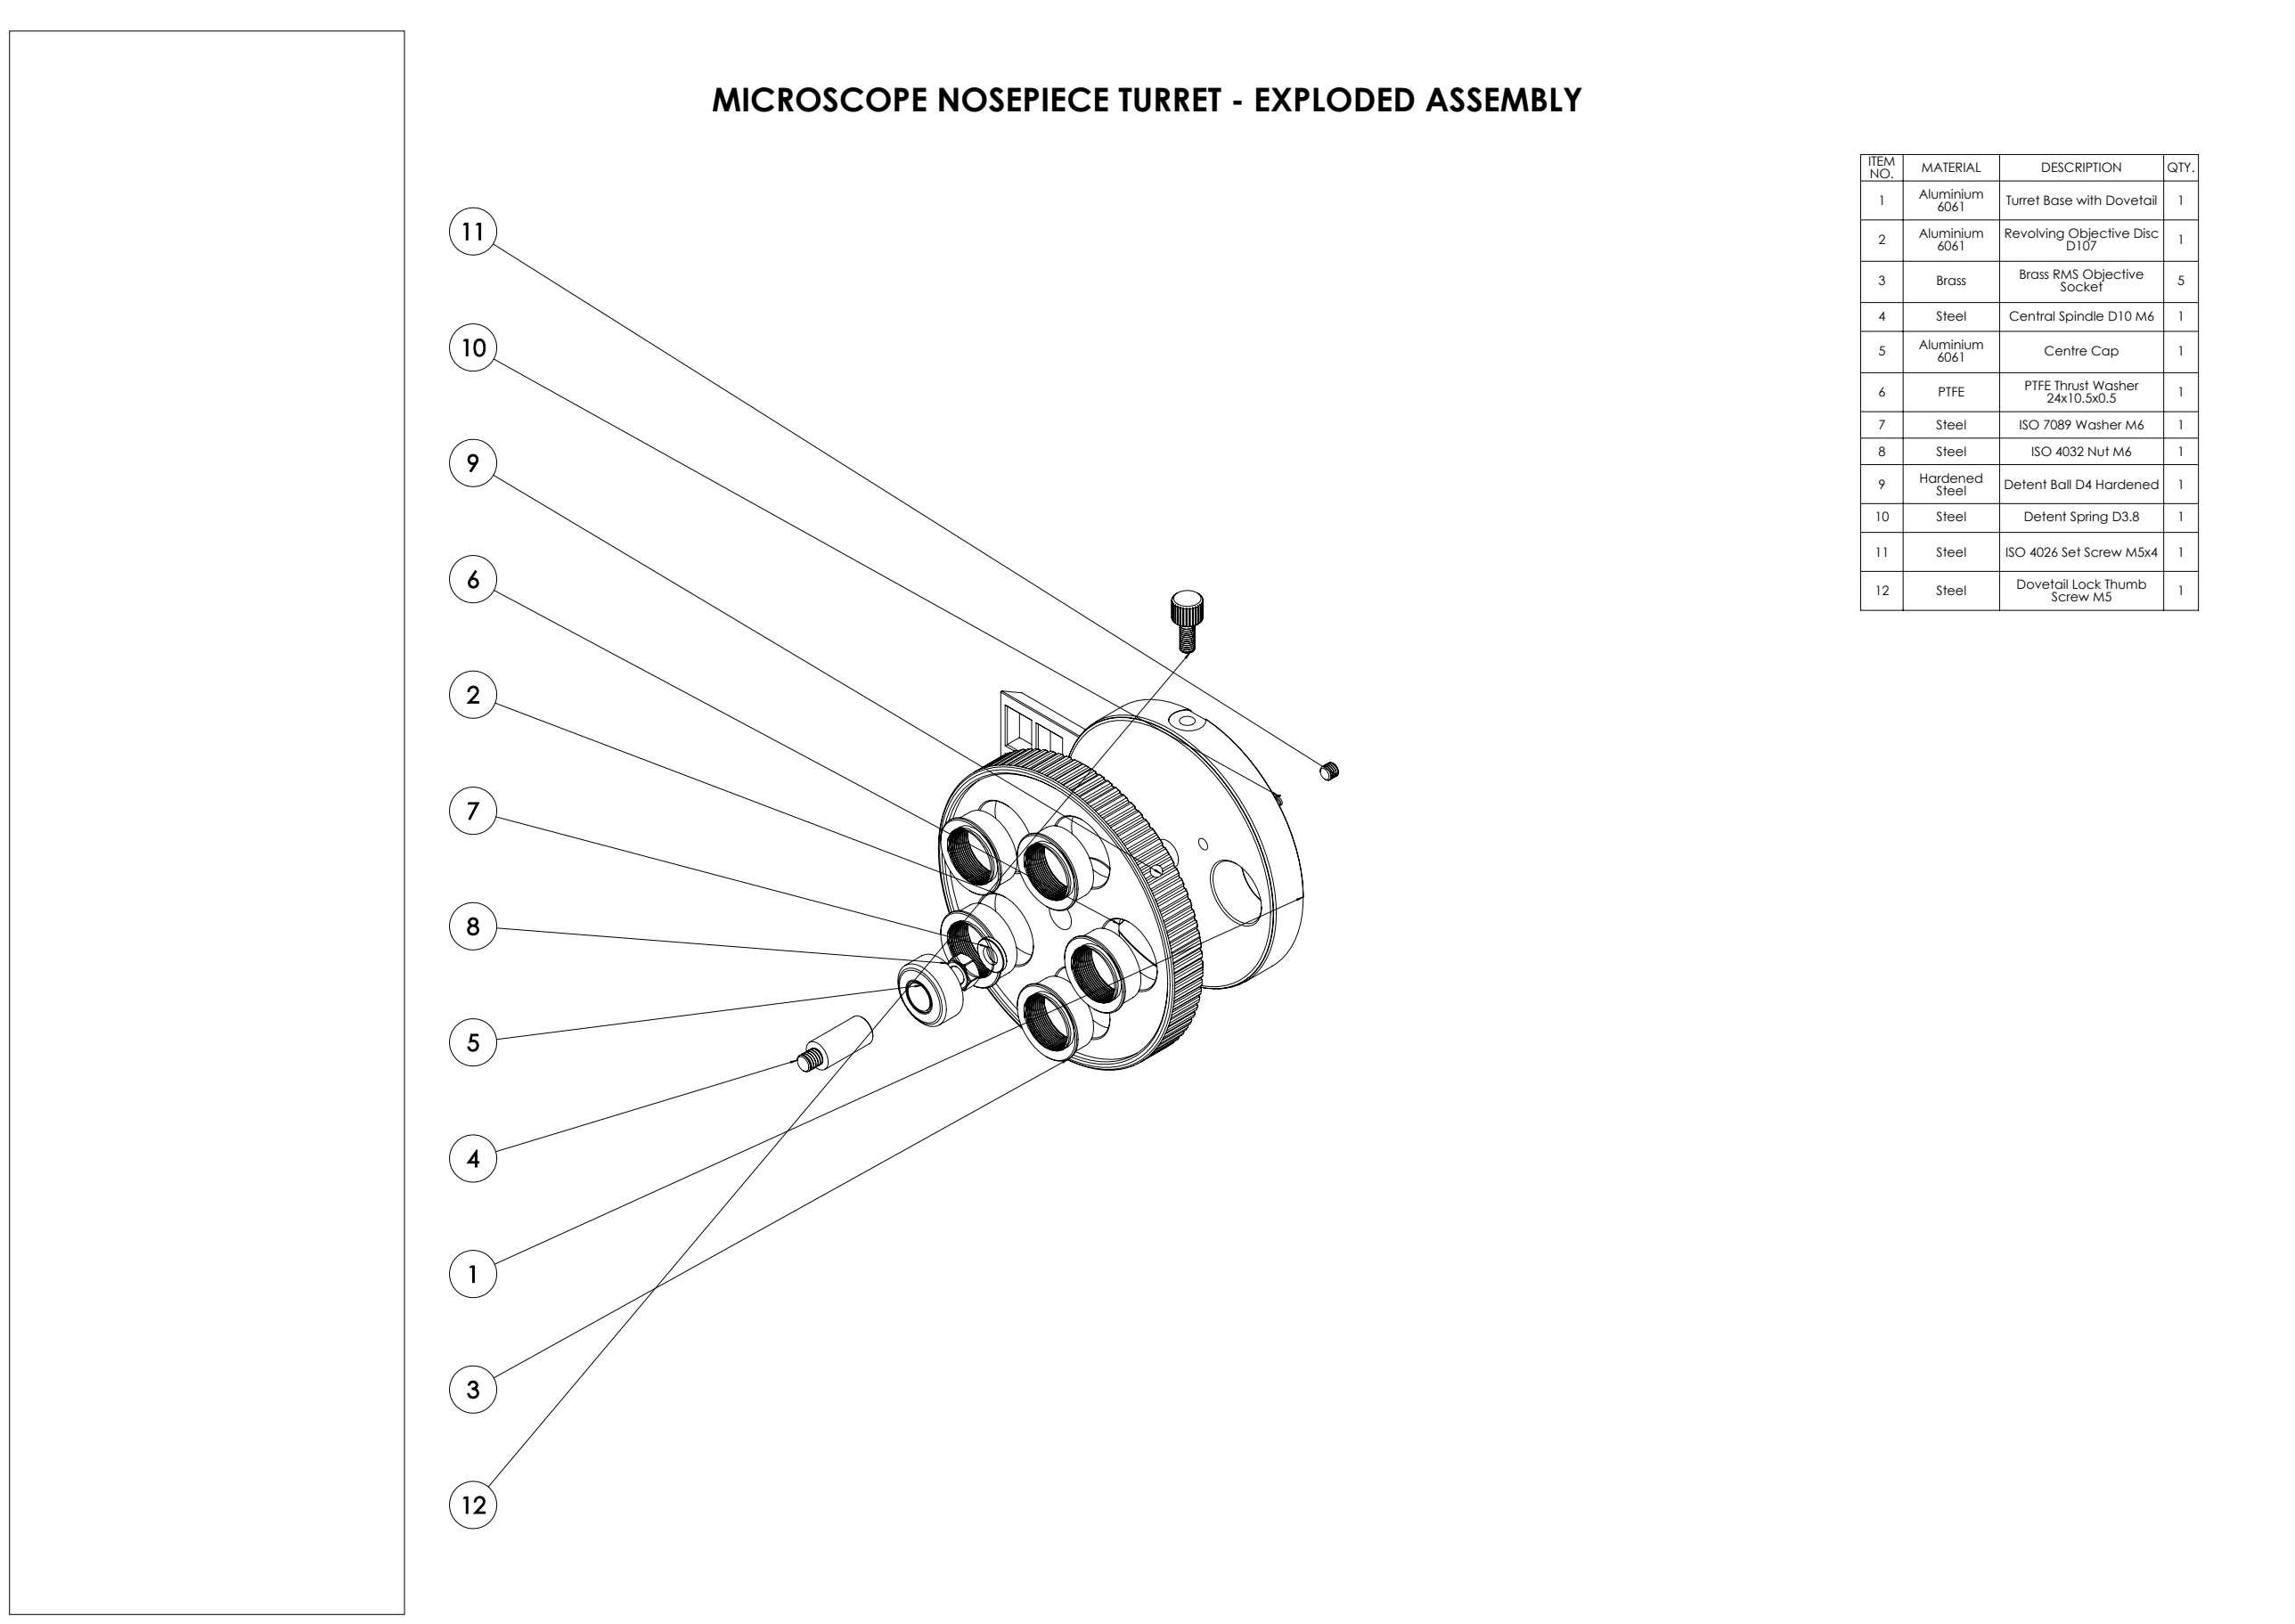
ISO-10303-21;
HEADER;
/* Generated by software containing ST-Developer
 * from STEP Tools, Inc. (www.steptools.com) 
 */

FILE_DESCRIPTION(
/* description */ (''),
/* implementation_level */ '2;1');

FILE_NAME(
/* name */ 'MAS-288',
/* time_stamp */ '2026-10-21T02:03:06-07:00',
/* author */ (''),
/* organization */ (''),
/* preprocessor_version */ 'ST-DEVELOPER v20.2',
/* originating_system */ 'Autodesk Translation Framework v15.15.0.0',
/* authorisation */ '');

FILE_SCHEMA (('AUTOMOTIVE_DESIGN { 1 0 10303 214 3 1 1 }'));
ENDSEC;

DATA;
#10=MECHANICAL_DESIGN_GEOMETRIC_PRESENTATION_REPRESENTATION('',(#115,#116,
#117,#118,#119,#120,#121,#122,#123,#124,#125,#126),#38528);
#11=ITEM_DEFINED_TRANSFORMATION($,$,#17218,#19009);
#12=ITEM_DEFINED_TRANSFORMATION($,$,#17323,#19010);
#13=ITEM_DEFINED_TRANSFORMATION($,$,#18599,#19011);
#14=ITEM_DEFINED_TRANSFORMATION($,$,#18599,#19012);
#15=ITEM_DEFINED_TRANSFORMATION($,$,#18599,#19013);
#16=ITEM_DEFINED_TRANSFORMATION($,$,#18599,#19014);
#17=ITEM_DEFINED_TRANSFORMATION($,$,#18599,#19015);
#18=ITEM_DEFINED_TRANSFORMATION($,$,#18641,#19016);
#19=ITEM_DEFINED_TRANSFORMATION($,$,#18673,#19017);
#20=ITEM_DEFINED_TRANSFORMATION($,$,#18699,#19018);
#21=ITEM_DEFINED_TRANSFORMATION($,$,#18708,#19019);
#22=ITEM_DEFINED_TRANSFORMATION($,$,#18722,#19020);
#23=ITEM_DEFINED_TRANSFORMATION($,$,#18766,#19021);
#24=ITEM_DEFINED_TRANSFORMATION($,$,#18769,#19022);
#25=ITEM_DEFINED_TRANSFORMATION($,$,#18774,#19023);
#26=ITEM_DEFINED_TRANSFORMATION($,$,#18808,#19024);
#27=(
REPRESENTATION_RELATIONSHIP($,$,#38576,#38575)
REPRESENTATION_RELATIONSHIP_WITH_TRANSFORMATION(#11)
SHAPE_REPRESENTATION_RELATIONSHIP()
);
#28=(
REPRESENTATION_RELATIONSHIP($,$,#38577,#38575)
REPRESENTATION_RELATIONSHIP_WITH_TRANSFORMATION(#12)
SHAPE_REPRESENTATION_RELATIONSHIP()
);
#29=(
REPRESENTATION_RELATIONSHIP($,$,#38578,#38575)
REPRESENTATION_RELATIONSHIP_WITH_TRANSFORMATION(#13)
SHAPE_REPRESENTATION_RELATIONSHIP()
);
#30=(
REPRESENTATION_RELATIONSHIP($,$,#38578,#38575)
REPRESENTATION_RELATIONSHIP_WITH_TRANSFORMATION(#14)
SHAPE_REPRESENTATION_RELATIONSHIP()
);
#31=(
REPRESENTATION_RELATIONSHIP($,$,#38578,#38575)
REPRESENTATION_RELATIONSHIP_WITH_TRANSFORMATION(#15)
SHAPE_REPRESENTATION_RELATIONSHIP()
);
#32=(
REPRESENTATION_RELATIONSHIP($,$,#38578,#38575)
REPRESENTATION_RELATIONSHIP_WITH_TRANSFORMATION(#16)
SHAPE_REPRESENTATION_RELATIONSHIP()
);
#33=(
REPRESENTATION_RELATIONSHIP($,$,#38578,#38575)
REPRESENTATION_RELATIONSHIP_WITH_TRANSFORMATION(#17)
SHAPE_REPRESENTATION_RELATIONSHIP()
);
#34=(
REPRESENTATION_RELATIONSHIP($,$,#38579,#38575)
REPRESENTATION_RELATIONSHIP_WITH_TRANSFORMATION(#18)
SHAPE_REPRESENTATION_RELATIONSHIP()
);
#35=(
REPRESENTATION_RELATIONSHIP($,$,#38580,#38575)
REPRESENTATION_RELATIONSHIP_WITH_TRANSFORMATION(#19)
SHAPE_REPRESENTATION_RELATIONSHIP()
);
#36=(
REPRESENTATION_RELATIONSHIP($,$,#38581,#38575)
REPRESENTATION_RELATIONSHIP_WITH_TRANSFORMATION(#20)
SHAPE_REPRESENTATION_RELATIONSHIP()
);
#37=(
REPRESENTATION_RELATIONSHIP($,$,#38582,#38575)
REPRESENTATION_RELATIONSHIP_WITH_TRANSFORMATION(#21)
SHAPE_REPRESENTATION_RELATIONSHIP()
);
#38=(
REPRESENTATION_RELATIONSHIP($,$,#38583,#38575)
REPRESENTATION_RELATIONSHIP_WITH_TRANSFORMATION(#22)
SHAPE_REPRESENTATION_RELATIONSHIP()
);
#39=(
REPRESENTATION_RELATIONSHIP($,$,#38584,#38575)
REPRESENTATION_RELATIONSHIP_WITH_TRANSFORMATION(#23)
SHAPE_REPRESENTATION_RELATIONSHIP()
);
#40=(
REPRESENTATION_RELATIONSHIP($,$,#38585,#38575)
REPRESENTATION_RELATIONSHIP_WITH_TRANSFORMATION(#24)
SHAPE_REPRESENTATION_RELATIONSHIP()
);
#41=(
REPRESENTATION_RELATIONSHIP($,$,#38586,#38575)
REPRESENTATION_RELATIONSHIP_WITH_TRANSFORMATION(#25)
SHAPE_REPRESENTATION_RELATIONSHIP()
);
#42=(
REPRESENTATION_RELATIONSHIP($,$,#38587,#38575)
REPRESENTATION_RELATIONSHIP_WITH_TRANSFORMATION(#26)
SHAPE_REPRESENTATION_RELATIONSHIP()
);
#43=CONTEXT_DEPENDENT_SHAPE_REPRESENTATION(#27,#38559);
#44=CONTEXT_DEPENDENT_SHAPE_REPRESENTATION(#28,#38560);
#45=CONTEXT_DEPENDENT_SHAPE_REPRESENTATION(#29,#38561);
#46=CONTEXT_DEPENDENT_SHAPE_REPRESENTATION(#30,#38562);
#47=CONTEXT_DEPENDENT_SHAPE_REPRESENTATION(#31,#38563);
#48=CONTEXT_DEPENDENT_SHAPE_REPRESENTATION(#32,#38564);
#49=CONTEXT_DEPENDENT_SHAPE_REPRESENTATION(#33,#38565);
#50=CONTEXT_DEPENDENT_SHAPE_REPRESENTATION(#34,#38566);
#51=CONTEXT_DEPENDENT_SHAPE_REPRESENTATION(#35,#38567);
#52=CONTEXT_DEPENDENT_SHAPE_REPRESENTATION(#36,#38568);
#53=CONTEXT_DEPENDENT_SHAPE_REPRESENTATION(#37,#38569);
#54=CONTEXT_DEPENDENT_SHAPE_REPRESENTATION(#38,#38570);
#55=CONTEXT_DEPENDENT_SHAPE_REPRESENTATION(#39,#38571);
#56=CONTEXT_DEPENDENT_SHAPE_REPRESENTATION(#40,#38572);
#57=CONTEXT_DEPENDENT_SHAPE_REPRESENTATION(#41,#38573);
#58=CONTEXT_DEPENDENT_SHAPE_REPRESENTATION(#42,#38574);
#59=NEXT_ASSEMBLY_USAGE_OCCURRENCE('01_Turret_Base_with_Dovetail:1',
'01_Turret_Base_with_Dovetail:1','01_Turret_Base_with_Dovetail:1',#38589,
#38590,'01_Turret_Base_with_Dovetail:1');
#60=NEXT_ASSEMBLY_USAGE_OCCURRENCE('02_Revolving_Objective_Disc_D107:1',
'02_Revolving_Objective_Disc_D107:1',
'02_Revolving_Objective_Disc_D107:1',#38589,#38591,
'02_Revolving_Objective_Disc_D107:1');
#61=NEXT_ASSEMBLY_USAGE_OCCURRENCE('03_Brass_RMS_Objective_Socket:2',
'03_Brass_RMS_Objective_Socket:2','03_Brass_RMS_Objective_Socket:2',#38589,
#38592,'03_Brass_RMS_Objective_Socket:2');
#62=NEXT_ASSEMBLY_USAGE_OCCURRENCE('03_Brass_RMS_Objective_Socket:3',
'03_Brass_RMS_Objective_Socket:3','03_Brass_RMS_Objective_Socket:3',#38589,
#38592,'03_Brass_RMS_Objective_Socket:3');
#63=NEXT_ASSEMBLY_USAGE_OCCURRENCE('03_Brass_RMS_Objective_Socket:4',
'03_Brass_RMS_Objective_Socket:4','03_Brass_RMS_Objective_Socket:4',#38589,
#38592,'03_Brass_RMS_Objective_Socket:4');
#64=NEXT_ASSEMBLY_USAGE_OCCURRENCE('03_Brass_RMS_Objective_Socket:5',
'03_Brass_RMS_Objective_Socket:5','03_Brass_RMS_Objective_Socket:5',#38589,
#38592,'03_Brass_RMS_Objective_Socket:5');
#65=NEXT_ASSEMBLY_USAGE_OCCURRENCE('03_Brass_RMS_Objective_Socket:6',
'03_Brass_RMS_Objective_Socket:6','03_Brass_RMS_Objective_Socket:6',#38589,
#38592,'03_Brass_RMS_Objective_Socket:6');
#66=NEXT_ASSEMBLY_USAGE_OCCURRENCE('04_Central_Spindle_D10_M6:2',
'04_Central_Spindle_D10_M6:2','04_Central_Spindle_D10_M6:2',#38589,#38593,
'04_Central_Spindle_D10_M6:2');
#67=NEXT_ASSEMBLY_USAGE_OCCURRENCE('05_Centre_Cap:2','05_Centre_Cap:2',
'05_Centre_Cap:2',#38589,#38594,'05_Centre_Cap:2');
#68=NEXT_ASSEMBLY_USAGE_OCCURRENCE(
'06_PTFE_Thrust_Washer_24x10.5x0.5:2',
'06_PTFE_Thrust_Washer_24x10.5x0.5:2',
'06_PTFE_Thrust_Washer_24x10.5x0.5:2',#38589,#38595,
'06_PTFE_Thrust_Washer_24x10.5x0.5:2');
#69=NEXT_ASSEMBLY_USAGE_OCCURRENCE('07_ISO_7089_Washer_M6:2',
'07_ISO_7089_Washer_M6:2','07_ISO_7089_Washer_M6:2',#38589,#38596,
'07_ISO_7089_Washer_M6:2');
#70=NEXT_ASSEMBLY_USAGE_OCCURRENCE('08_ISO_4032_Nut_M6:2',
'08_ISO_4032_Nut_M6:2','08_ISO_4032_Nut_M6:2',#38589,#38597,
'08_ISO_4032_Nut_M6:2');
#71=NEXT_ASSEMBLY_USAGE_OCCURRENCE('09_Detent_Ball_D4_Hardened:2',
'09_Detent_Ball_D4_Hardened:2','09_Detent_Ball_D4_Hardened:2',#38589,#38598,
'09_Detent_Ball_D4_Hardened:2');
#72=NEXT_ASSEMBLY_USAGE_OCCURRENCE('10_Detent_Spring_D3.8:2',
'10_Detent_Spring_D3.8:2','10_Detent_Spring_D3.8:2',#38589,#38599,
'10_Detent_Spring_D3.8:2');
#73=NEXT_ASSEMBLY_USAGE_OCCURRENCE('11_ISO_4026_Set_Screw_M5x4:2',
'11_ISO_4026_Set_Screw_M5x4:2','11_ISO_4026_Set_Screw_M5x4:2',#38589,#38600,
'11_ISO_4026_Set_Screw_M5x4:2');
#74=NEXT_ASSEMBLY_USAGE_OCCURRENCE('12_Dovetail_Lock_Thumb_Screw_M5:2',
'12_Dovetail_Lock_Thumb_Screw_M5:2','12_Dovetail_Lock_Thumb_Screw_M5:2',
#38589,#38601,'12_Dovetail_Lock_Thumb_Screw_M5:2');
#75=SPHERICAL_SURFACE('',#18767,2.);
#76=B_SPLINE_SURFACE_WITH_KNOTS('',3,3,((#30041,#30042,#30043,#30044,#30045,
#30046,#30047,#30048,#30049,#30050,#30051,#30052,#30053,#30054,#30055,#30056,
#30057,#30058,#30059,#30060,#30061,#30062,#30063,#30064,#30065,#30066,#30067,
#30068,#30069,#30070,#30071,#30072,#30073,#30074,#30075,#30076,#30077,#30078,
#30079,#30080,#30081,#30082,#30083,#30084,#30085,#30086,#30087,#30088,#30089,
#30090,#30091,#30092,#30093,#30094,#30095,#30096,#30097,#30098,#30099,#30100,
#30101,#30102,#30103,#30104,#30105,#30106,#30107,#30108,#30109,#30110,#30111,
#30112,#30113,#30114,#30115,#30116,#30117,#30118,#30119,#30120,#30121,#30122,
#30123,#30124,#30125,#30126,#30127,#30128,#30129,#30130,#30131,#30132,#30133,
#30134,#30135,#30136,#30137,#30138,#30139,#30140,#30141,#30142,#30143,#30144,
#30145,#30146,#30147,#30148,#30149,#30150,#30151,#30152,#30153,#30154,#30155,
#30156,#30157,#30158,#30159,#30160,#30161,#30162,#30163,#30164,#30165,#30166,
#30167,#30168,#30169,#30170,#30171,#30172,#30173,#30174,#30175,#30176,#30177,
#30178,#30179,#30180,#30181,#30182,#30183,#30184,#30185,#30186,#30187,#30188,
#30189,#30190,#30191,#30192,#30193,#30194,#30195,#30196,#30197,#30198,#30199),
(#30200,#30201,#30202,#30203,#30204,#30205,#30206,#30207,#30208,#30209,
#30210,#30211,#30212,#30213,#30214,#30215,#30216,#30217,#30218,#30219,#30220,
#30221,#30222,#30223,#30224,#30225,#30226,#30227,#30228,#30229,#30230,#30231,
#30232,#30233,#30234,#30235,#30236,#30237,#30238,#30239,#30240,#30241,#30242,
#30243,#30244,#30245,#30246,#30247,#30248,#30249,#30250,#30251,#30252,#30253,
#30254,#30255,#30256,#30257,#30258,#30259,#30260,#30261,#30262,#30263,#30264,
#30265,#30266,#30267,#30268,#30269,#30270,#30271,#30272,#30273,#30274,#30275,
#30276,#30277,#30278,#30279,#30280,#30281,#30282,#30283,#30284,#30285,#30286,
#30287,#30288,#30289,#30290,#30291,#30292,#30293,#30294,#30295,#30296,#30297,
#30298,#30299,#30300,#30301,#30302,#30303,#30304,#30305,#30306,#30307,#30308,
#30309,#30310,#30311,#30312,#30313,#30314,#30315,#30316,#30317,#30318,#30319,
#30320,#30321,#30322,#30323,#30324,#30325,#30326,#30327,#30328,#30329,#30330,
#30331,#30332,#30333,#30334,#30335,#30336,#30337,#30338,#30339,#30340,#30341,
#30342,#30343,#30344,#30345,#30346,#30347,#30348,#30349,#30350,#30351,#30352,
#30353,#30354,#30355,#30356,#30357,#30358),(#30359,#30360,#30361,#30362,
#30363,#30364,#30365,#30366,#30367,#30368,#30369,#30370,#30371,#30372,#30373,
#30374,#30375,#30376,#30377,#30378,#30379,#30380,#30381,#30382,#30383,#30384,
#30385,#30386,#30387,#30388,#30389,#30390,#30391,#30392,#30393,#30394,#30395,
#30396,#30397,#30398,#30399,#30400,#30401,#30402,#30403,#30404,#30405,#30406,
#30407,#30408,#30409,#30410,#30411,#30412,#30413,#30414,#30415,#30416,#30417,
#30418,#30419,#30420,#30421,#30422,#30423,#30424,#30425,#30426,#30427,#30428,
#30429,#30430,#30431,#30432,#30433,#30434,#30435,#30436,#30437,#30438,#30439,
#30440,#30441,#30442,#30443,#30444,#30445,#30446,#30447,#30448,#30449,#30450,
#30451,#30452,#30453,#30454,#30455,#30456,#30457,#30458,#30459,#30460,#30461,
#30462,#30463,#30464,#30465,#30466,#30467,#30468,#30469,#30470,#30471,#30472,
#30473,#30474,#30475,#30476,#30477,#30478,#30479,#30480,#30481,#30482,#30483,
#30484,#30485,#30486,#30487,#30488,#30489,#30490,#30491,#30492,#30493,#30494,
#30495,#30496,#30497,#30498,#30499,#30500,#30501,#30502,#30503,#30504,#30505,
#30506,#30507,#30508,#30509,#30510,#30511,#30512,#30513,#30514,#30515,#30516,
#30517),(#30518,#30519,#30520,#30521,#30522,#30523,#30524,#30525,#30526,
#30527,#30528,#30529,#30530,#30531,#30532,#30533,#30534,#30535,#30536,#30537,
#30538,#30539,#30540,#30541,#30542,#30543,#30544,#30545,#30546,#30547,#30548,
#30549,#30550,#30551,#30552,#30553,#30554,#30555,#30556,#30557,#30558,#30559,
#30560,#30561,#30562,#30563,#30564,#30565,#30566,#30567,#30568,#30569,#30570,
#30571,#30572,#30573,#30574,#30575,#30576,#30577,#30578,#30579,#30580,#30581,
#30582,#30583,#30584,#30585,#30586,#30587,#30588,#30589,#30590,#30591,#30592,
#30593,#30594,#30595,#30596,#30597,#30598,#30599,#30600,#30601,#30602,#30603,
#30604,#30605,#30606,#30607,#30608,#30609,#30610,#30611,#30612,#30613,#30614,
#30615,#30616,#30617,#30618,#30619,#30620,#30621,#30622,#30623,#30624,#30625,
#30626,#30627,#30628,#30629,#30630,#30631,#30632,#30633,#30634,#30635,#30636,
#30637,#30638,#30639,#30640,#30641,#30642,#30643,#30644,#30645,#30646,#30647,
#30648,#30649,#30650,#30651,#30652,#30653,#30654,#30655,#30656,#30657,#30658,
#30659,#30660,#30661,#30662,#30663,#30664,#30665,#30666,#30667,#30668,#30669,
#30670,#30671,#30672,#30673,#30674,#30675,#30676)),.UNSPECIFIED.,.F.,.F.,
 .F.,(4,4),(4,1,1,1,1,1,1,1,1,1,1,1,1,1,1,1,1,1,1,1,1,1,1,1,1,1,1,1,1,1,
1,1,1,1,1,1,1,1,1,1,1,1,1,1,1,1,1,1,1,1,1,1,1,1,1,1,1,1,1,1,1,1,1,1,1,1,
1,1,1,1,1,1,1,1,1,1,1,1,1,1,1,1,1,1,1,1,1,1,1,1,1,1,1,1,1,1,1,1,1,1,1,1,
1,1,1,1,1,1,1,1,1,1,1,1,1,1,1,1,1,1,1,1,1,1,1,1,1,1,1,1,1,1,1,1,1,1,1,1,
1,1,1,1,1,1,1,1,1,1,1,1,1,1,1,1,1,1,4),(0.,0.0485551576388473),(11.8415763884111,
12.3379359869576,12.8342955855041,13.3306551840506,13.827014782597,14.3233743811435,
14.81973397969,15.3160935782364,15.8124531767829,16.3088127753294,16.8051723738759,
17.3015319724223,17.7978915709688,18.2942511695153,18.7906107680618,19.2869703666082,
19.7833299651547,20.2796895637012,20.7760491622476,21.2724087607941,21.7687683593406,
22.2651279578871,22.7614875564335,23.25784715498,23.7542067535265,24.2505663520729,
24.7469259506194,25.2432855491659,25.7396451477124,26.2360047462588,26.7323643448053,
27.2287239433518,27.7250835418983,28.2214431404447,28.7178027389912,29.2141623375377,
29.7105219360841,30.2068815346306,30.7032411331771,31.1996007317236,31.69596033027,
32.1923199288165,32.688679527363,33.1850391259094,33.6813987244559,34.1777583230024,
34.6741179215489,35.1704775200953,35.6668371186418,36.1631967171883,36.6595563157347,
37.1559159142812,37.6522755128277,38.1486351113742,38.6449947099206,39.1413543084671,
39.6377139070136,40.1340735055601,40.6304331041065,41.126792702653,41.6231523011995,
42.1195118997459,42.6158714982924,43.1122310968389,43.6085906953854,44.1049502939318,
44.6013098924783,45.0976694910248,45.5940290895712,46.0903886881177,46.5867482866642,
47.0831078852107,47.5794674837571,48.0758270823036,48.5721866808501,49.0685462793965,
49.564905877943,50.0612654764895,50.557625075036,51.0539846735824,51.5503442721289,
52.0467038706754,52.5430634692219,53.0394230677683,53.5357826663148,54.0321422648613,
54.5285018634077,55.0248614619542,55.5212210605007,56.0175806590472,56.5139402575936,
57.0102998561401,57.5066594546866,58.003019053233,58.4993786517795,58.995738250326,
59.4920978488725,59.9884574474189,60.4848170459654,60.9811766445119,61.4775362430584,
61.9738958416048,62.4702554401513,62.9666150386978,63.4629746372442,63.9593342357907,
64.4556938343372,64.9520534328837,65.4484130314301,65.9447726299766,66.4411322285231,
66.9374918270696,67.433851425616,67.9302110241625,68.426570622709,68.9229302212554,
69.4192898198019,69.9156494183484,70.4120090168948,70.9083686154413,71.4047282139878,
71.9010878125343,72.3974474110807,72.8938070096272,73.3901666081737,73.8865262067201,
74.3828858052666,74.8792454038131,75.3756050023596,75.871964600906,76.3683241994525,
76.864683797999,77.3610433965455,77.8574029950919,78.3537625936384,78.8501221921849,
79.3464817907313,79.8428413892778,80.3392009878243,80.8355605863708,81.3319201849172,
81.8282797834637,82.3246393820102,82.8209989805567,83.3173585791031,83.8137181776496,
84.3100777761961,84.8064373747425,85.302796973289,85.7991565718355,86.295516170382,
86.7918757689284,87.2882353674749,87.7845949660214,88.2809545645678,88.7773141631143,
89.2736737616608),.UNSPECIFIED.);
#77=B_SPLINE_SURFACE_WITH_KNOTS('',3,3,((#30959,#30960,#30961,#30962,#30963,
#30964,#30965,#30966,#30967,#30968,#30969,#30970,#30971,#30972,#30973,#30974,
#30975,#30976,#30977,#30978,#30979,#30980,#30981,#30982,#30983,#30984,#30985,
#30986,#30987,#30988,#30989,#30990,#30991,#30992,#30993,#30994,#30995,#30996,
#30997,#30998,#30999,#31000,#31001,#31002,#31003,#31004,#31005,#31006,#31007,
#31008,#31009,#31010,#31011,#31012,#31013,#31014,#31015,#31016,#31017,#31018,
#31019,#31020,#31021,#31022,#31023,#31024,#31025,#31026,#31027,#31028,#31029,
#31030,#31031,#31032,#31033,#31034,#31035,#31036,#31037,#31038,#31039,#31040,
#31041,#31042,#31043,#31044,#31045,#31046,#31047,#31048,#31049,#31050,#31051,
#31052,#31053,#31054,#31055,#31056,#31057,#31058,#31059,#31060,#31061,#31062,
#31063,#31064,#31065,#31066,#31067,#31068,#31069,#31070,#31071,#31072,#31073,
#31074,#31075,#31076,#31077,#31078,#31079,#31080,#31081,#31082,#31083,#31084,
#31085,#31086,#31087,#31088,#31089,#31090,#31091,#31092,#31093,#31094,#31095,
#31096,#31097,#31098,#31099,#31100,#31101,#31102,#31103,#31104,#31105,#31106,
#31107,#31108,#31109,#31110,#31111,#31112,#31113,#31114,#31115,#31116,#31117),
(#31118,#31119,#31120,#31121,#31122,#31123,#31124,#31125,#31126,#31127,
#31128,#31129,#31130,#31131,#31132,#31133,#31134,#31135,#31136,#31137,#31138,
#31139,#31140,#31141,#31142,#31143,#31144,#31145,#31146,#31147,#31148,#31149,
#31150,#31151,#31152,#31153,#31154,#31155,#31156,#31157,#31158,#31159,#31160,
#31161,#31162,#31163,#31164,#31165,#31166,#31167,#31168,#31169,#31170,#31171,
#31172,#31173,#31174,#31175,#31176,#31177,#31178,#31179,#31180,#31181,#31182,
#31183,#31184,#31185,#31186,#31187,#31188,#31189,#31190,#31191,#31192,#31193,
#31194,#31195,#31196,#31197,#31198,#31199,#31200,#31201,#31202,#31203,#31204,
#31205,#31206,#31207,#31208,#31209,#31210,#31211,#31212,#31213,#31214,#31215,
#31216,#31217,#31218,#31219,#31220,#31221,#31222,#31223,#31224,#31225,#31226,
#31227,#31228,#31229,#31230,#31231,#31232,#31233,#31234,#31235,#31236,#31237,
#31238,#31239,#31240,#31241,#31242,#31243,#31244,#31245,#31246,#31247,#31248,
#31249,#31250,#31251,#31252,#31253,#31254,#31255,#31256,#31257,#31258,#31259,
#31260,#31261,#31262,#31263,#31264,#31265,#31266,#31267,#31268,#31269,#31270,
#31271,#31272,#31273,#31274,#31275,#31276),(#31277,#31278,#31279,#31280,
#31281,#31282,#31283,#31284,#31285,#31286,#31287,#31288,#31289,#31290,#31291,
#31292,#31293,#31294,#31295,#31296,#31297,#31298,#31299,#31300,#31301,#31302,
#31303,#31304,#31305,#31306,#31307,#31308,#31309,#31310,#31311,#31312,#31313,
#31314,#31315,#31316,#31317,#31318,#31319,#31320,#31321,#31322,#31323,#31324,
#31325,#31326,#31327,#31328,#31329,#31330,#31331,#31332,#31333,#31334,#31335,
#31336,#31337,#31338,#31339,#31340,#31341,#31342,#31343,#31344,#31345,#31346,
#31347,#31348,#31349,#31350,#31351,#31352,#31353,#31354,#31355,#31356,#31357,
#31358,#31359,#31360,#31361,#31362,#31363,#31364,#31365,#31366,#31367,#31368,
#31369,#31370,#31371,#31372,#31373,#31374,#31375,#31376,#31377,#31378,#31379,
#31380,#31381,#31382,#31383,#31384,#31385,#31386,#31387,#31388,#31389,#31390,
#31391,#31392,#31393,#31394,#31395,#31396,#31397,#31398,#31399,#31400,#31401,
#31402,#31403,#31404,#31405,#31406,#31407,#31408,#31409,#31410,#31411,#31412,
#31413,#31414,#31415,#31416,#31417,#31418,#31419,#31420,#31421,#31422,#31423,
#31424,#31425,#31426,#31427,#31428,#31429,#31430,#31431,#31432,#31433,#31434,
#31435),(#31436,#31437,#31438,#31439,#31440,#31441,#31442,#31443,#31444,
#31445,#31446,#31447,#31448,#31449,#31450,#31451,#31452,#31453,#31454,#31455,
#31456,#31457,#31458,#31459,#31460,#31461,#31462,#31463,#31464,#31465,#31466,
#31467,#31468,#31469,#31470,#31471,#31472,#31473,#31474,#31475,#31476,#31477,
#31478,#31479,#31480,#31481,#31482,#31483,#31484,#31485,#31486,#31487,#31488,
#31489,#31490,#31491,#31492,#31493,#31494,#31495,#31496,#31497,#31498,#31499,
#31500,#31501,#31502,#31503,#31504,#31505,#31506,#31507,#31508,#31509,#31510,
#31511,#31512,#31513,#31514,#31515,#31516,#31517,#31518,#31519,#31520,#31521,
#31522,#31523,#31524,#31525,#31526,#31527,#31528,#31529,#31530,#31531,#31532,
#31533,#31534,#31535,#31536,#31537,#31538,#31539,#31540,#31541,#31542,#31543,
#31544,#31545,#31546,#31547,#31548,#31549,#31550,#31551,#31552,#31553,#31554,
#31555,#31556,#31557,#31558,#31559,#31560,#31561,#31562,#31563,#31564,#31565,
#31566,#31567,#31568,#31569,#31570,#31571,#31572,#31573,#31574,#31575,#31576,
#31577,#31578,#31579,#31580,#31581,#31582,#31583,#31584,#31585,#31586,#31587,
#31588,#31589,#31590,#31591,#31592,#31593,#31594)),.UNSPECIFIED.,.F.,.F.,
 .F.,(4,4),(4,1,1,1,1,1,1,1,1,1,1,1,1,1,1,1,1,1,1,1,1,1,1,1,1,1,1,1,1,1,
1,1,1,1,1,1,1,1,1,1,1,1,1,1,1,1,1,1,1,1,1,1,1,1,1,1,1,1,1,1,1,1,1,1,1,1,
1,1,1,1,1,1,1,1,1,1,1,1,1,1,1,1,1,1,1,1,1,1,1,1,1,1,1,1,1,1,1,1,1,1,1,1,
1,1,1,1,1,1,1,1,1,1,1,1,1,1,1,1,1,1,1,1,1,1,1,1,1,1,1,1,1,1,1,1,1,1,1,1,
1,1,1,1,1,1,1,1,1,1,1,1,1,1,1,1,1,1,4),(0.,0.0485551576388473),(14.3988838068023,
14.8952434053488,15.3916030038952,15.8879626024417,16.3843222009882,16.8806817995346,
17.3770413980811,17.8734009966276,18.3697605951741,18.8661201937205,19.362479792267,
19.8588393908135,20.3551989893599,20.8515585879064,21.3479181864529,21.8442777849994,
22.3406373835458,22.8369969820923,23.3333565806388,23.8297161791853,24.3260757777317,
24.8224353762782,25.3187949748247,25.8151545733711,26.3115141719176,26.8078737704641,
27.3042333690106,27.800592967557,28.2969525661035,28.79331216465,29.2896717631964,
29.7860313617429,30.2823909602894,30.7787505588359,31.2751101573823,31.7714697559288,
32.2678293544753,32.7641889530218,33.2605485515682,33.7569081501147,34.2532677486612,
34.7496273472076,35.2459869457541,35.7423465443006,36.2387061428471,36.7350657413935,
37.23142533994,37.7277849384865,38.2241445370329,38.7205041355794,39.2168637341259,
39.7132233326724,40.2095829312188,40.7059425297653,41.2023021283118,41.6986617268582,
42.1950213254047,42.6913809239512,43.1877405224977,43.6841001210441,44.1804597195906,
44.6768193181371,45.1731789166836,45.66953851523,46.1658981137765,46.662257712323,
47.1586173108694,47.6549769094159,48.1513365079624,48.6476961065089,49.1440557050553,
49.6404153036018,50.1367749021483,50.6331345006947,51.1294940992412,51.6258536977877,
52.1222132963342,52.6185728948806,53.1149324934271,53.6112920919736,54.1076516905201,
54.6040112890665,55.100370887613,55.5967304861595,56.0930900847059,56.5894496832524,
57.0858092817989,57.5821688803454,58.0785284788918,58.5748880774383,59.0712476759848,
59.5676072745312,60.0639668730777,60.5603264716242,61.0566860701707,61.5530456687171,
62.0494052672636,62.5457648658101,63.0421244643565,63.538484062903,64.0348436614495,
64.531203259996,65.0275628585424,65.5239224570889,66.0202820556354,66.5166416541819,
67.0130012527283,67.5093608512748,68.0057204498213,68.5020800483677,68.9984396469142,
69.4947992454607,69.9911588440072,70.4875184425536,70.9838780411001,71.4802376396466,
71.9765972381931,72.4729568367395,72.969316435286,73.4656760338325,73.9620356323789,
74.4583952309254,74.9547548294719,75.4511144280183,75.9474740265648,76.4438336251113,
76.9401932236578,77.4365528222042,77.9329124207507,78.4292720192972,78.9256316178437,
79.4219912163901,79.9183508149366,80.4147104134831,80.9110700120296,81.407429610576,
81.9037892091225,82.400148807669,82.8965084062154,83.3928680047619,83.8892276033084,
84.3855872018549,84.8819468004013,85.3783063989478,85.8746659974943,86.3710255960407,
86.8673851945872,87.3637447931337,87.8601043916802,88.3564639902266,88.8528235887731,
89.3491831873196,89.845542785866,90.3419023844125,90.838261982959,91.3346215815055,
91.8309811800519),.UNSPECIFIED.);
#78=B_SPLINE_SURFACE_WITH_KNOTS('',3,3,((#32507,#32508,#32509,#32510,#32511,
#32512,#32513,#32514,#32515,#32516,#32517,#32518,#32519,#32520,#32521,#32522,
#32523,#32524,#32525,#32526,#32527,#32528,#32529,#32530,#32531,#32532,#32533,
#32534,#32535,#32536,#32537,#32538,#32539,#32540,#32541,#32542,#32543,#32544,
#32545,#32546,#32547,#32548,#32549,#32550),(#32551,#32552,#32553,#32554,
#32555,#32556,#32557,#32558,#32559,#32560,#32561,#32562,#32563,#32564,#32565,
#32566,#32567,#32568,#32569,#32570,#32571,#32572,#32573,#32574,#32575,#32576,
#32577,#32578,#32579,#32580,#32581,#32582,#32583,#32584,#32585,#32586,#32587,
#32588,#32589,#32590,#32591,#32592,#32593,#32594),(#32595,#32596,#32597,
#32598,#32599,#32600,#32601,#32602,#32603,#32604,#32605,#32606,#32607,#32608,
#32609,#32610,#32611,#32612,#32613,#32614,#32615,#32616,#32617,#32618,#32619,
#32620,#32621,#32622,#32623,#32624,#32625,#32626,#32627,#32628,#32629,#32630,
#32631,#32632,#32633,#32634,#32635,#32636,#32637,#32638),(#32639,#32640,
#32641,#32642,#32643,#32644,#32645,#32646,#32647,#32648,#32649,#32650,#32651,
#32652,#32653,#32654,#32655,#32656,#32657,#32658,#32659,#32660,#32661,#32662,
#32663,#32664,#32665,#32666,#32667,#32668,#32669,#32670,#32671,#32672,#32673,
#32674,#32675,#32676,#32677,#32678,#32679,#32680,#32681,#32682)),
 .UNSPECIFIED.,.F.,.F.,.F.,(4,4),(4,1,1,1,1,1,1,1,1,1,1,1,1,1,1,1,1,1,1,
1,1,1,1,1,1,1,1,1,1,1,1,1,1,1,1,1,1,1,1,1,1,4),(0.,0.0658467982010769),
(8.30747755240109,9.28631108327433,10.2651446141476,11.2439781450208,12.2228116758941,
13.2016452067673,14.1804787376406,15.1593122685138,16.1381457993871,17.1169793302603,
18.0958128611336,19.0746463920068,20.05347992288,21.0323134537533,22.0111469846265,
22.9899805154998,23.968814046373,24.9476475772463,25.9264811081195,26.9053146389928,
27.884148169866,28.8629817007393,29.8418152316125,30.8206487624858,31.799482293359,
32.7783158242323,33.7571493551055,34.7359828859787,35.714816416852,36.6936499477252,
37.6724834785985,38.6513170094717,39.630150540345,40.6089840712182,41.5878176020915,
42.5666511329647,43.545484663838,44.5243181947112,45.5031517255845,46.4819852564577,
47.460818787331,48.4396523182042),.UNSPECIFIED.);
#79=B_SPLINE_SURFACE_WITH_KNOTS('',3,3,((#32811,#32812,#32813,#32814,#32815,
#32816,#32817,#32818,#32819,#32820,#32821,#32822,#32823,#32824,#32825,#32826,
#32827,#32828,#32829,#32830,#32831,#32832,#32833,#32834,#32835,#32836,#32837,
#32838,#32839,#32840,#32841,#32842,#32843,#32844,#32845,#32846,#32847,#32848,
#32849,#32850,#32851,#32852,#32853,#32854),(#32855,#32856,#32857,#32858,
#32859,#32860,#32861,#32862,#32863,#32864,#32865,#32866,#32867,#32868,#32869,
#32870,#32871,#32872,#32873,#32874,#32875,#32876,#32877,#32878,#32879,#32880,
#32881,#32882,#32883,#32884,#32885,#32886,#32887,#32888,#32889,#32890,#32891,
#32892,#32893,#32894,#32895,#32896,#32897,#32898),(#32899,#32900,#32901,
#32902,#32903,#32904,#32905,#32906,#32907,#32908,#32909,#32910,#32911,#32912,
#32913,#32914,#32915,#32916,#32917,#32918,#32919,#32920,#32921,#32922,#32923,
#32924,#32925,#32926,#32927,#32928,#32929,#32930,#32931,#32932,#32933,#32934,
#32935,#32936,#32937,#32938,#32939,#32940,#32941,#32942),(#32943,#32944,
#32945,#32946,#32947,#32948,#32949,#32950,#32951,#32952,#32953,#32954,#32955,
#32956,#32957,#32958,#32959,#32960,#32961,#32962,#32963,#32964,#32965,#32966,
#32967,#32968,#32969,#32970,#32971,#32972,#32973,#32974,#32975,#32976,#32977,
#32978,#32979,#32980,#32981,#32982,#32983,#32984,#32985,#32986)),
 .UNSPECIFIED.,.F.,.F.,.F.,(4,4),(4,1,1,1,1,1,1,1,1,1,1,1,1,1,1,1,1,1,1,
1,1,1,1,1,1,1,1,1,1,1,1,1,1,1,1,1,1,1,1,1,1,4),(0.,0.0658467982010769),
(11.6150328478183,12.5938663786915,13.5726999095648,14.551533440438,15.5303669713113,
16.5092005021845,17.4880340330578,18.466867563931,19.4457010948043,20.4245346256775,
21.4033681565508,22.382201687424,23.3610352182973,24.3398687491705,25.3187022800437,
26.297535810917,27.2763693417902,28.2552028726635,29.2340364035367,30.21286993441,
31.1917034652832,32.1705369961565,33.1493705270297,34.128204057903,35.1070375887762,
36.0858711196495,37.0647046505227,38.043538181396,39.0223717122692,40.0012052431424,
40.9800387740157,41.9588723048889,42.9377058357622,43.9165393666354,44.8953728975087,
45.8742064283819,46.8530399592552,47.8318734901284,48.8107070210017,49.7895405518749,
50.7683740827482,51.7472076136214),.UNSPECIFIED.);
#80=B_SPLINE_SURFACE_WITH_KNOTS('',3,3,((#33437,#33438,#33439,#33440,#33441),
(#33442,#33443,#33444,#33445,#33446),(#33447,#33448,#33449,#33450,#33451),
(#33452,#33453,#33454,#33455,#33456)),.UNSPECIFIED.,.F.,.F.,.F.,(4,4),(4,
1,4),(0.,1.),(0.0610870649866808,0.309114526274187,0.639817807990862),
 .UNSPECIFIED.);
#81=B_SPLINE_SURFACE_WITH_KNOTS('',3,3,((#33486,#33487,#33488,#33489,#33490),
(#33491,#33492,#33493,#33494,#33495),(#33496,#33497,#33498,#33499,#33500),
(#33501,#33502,#33503,#33504,#33505)),.UNSPECIFIED.,.F.,.F.,.F.,(4,4),(4,
1,4),(0.,1.),(0.0610870649866807,0.309114526274187,0.639817807990862),
 .UNSPECIFIED.);
#82=B_SPLINE_SURFACE_WITH_KNOTS('',3,3,((#33575,#33576,#33577,#33578,#33579),
(#33580,#33581,#33582,#33583,#33584),(#33585,#33586,#33587,#33588,#33589),
(#33590,#33591,#33592,#33593,#33594)),.UNSPECIFIED.,.F.,.F.,.F.,(4,4),(4,
1,4),(0.,1.),(0.061087064986681,0.309114526274187,0.639817807990862),
 .UNSPECIFIED.);
#83=B_SPLINE_SURFACE_WITH_KNOTS('',3,3,((#33668,#33669,#33670,#33671,#33672),
(#33673,#33674,#33675,#33676,#33677),(#33678,#33679,#33680,#33681,#33682),
(#33683,#33684,#33685,#33686,#33687)),.UNSPECIFIED.,.F.,.F.,.F.,(4,4),(4,
1,4),(0.,1.),(0.0610870649866801,0.309114526274187,0.639817807990862),
 .UNSPECIFIED.);
#84=B_SPLINE_SURFACE_WITH_KNOTS('',3,3,((#33701,#33702,#33703,#33704,#33705),
(#33706,#33707,#33708,#33709,#33710),(#33711,#33712,#33713,#33714,#33715),
(#33716,#33717,#33718,#33719,#33720)),.UNSPECIFIED.,.F.,.F.,.F.,(4,4),(4,
1,4),(0.,1.),(0.0610870649866807,0.391790346703356,0.639817807990862),
 .UNSPECIFIED.);
#85=B_SPLINE_SURFACE_WITH_KNOTS('',3,3,((#33742,#33743,#33744,#33745,#33746),
(#33747,#33748,#33749,#33750,#33751),(#33752,#33753,#33754,#33755,#33756),
(#33757,#33758,#33759,#33760,#33761)),.UNSPECIFIED.,.F.,.F.,.F.,(4,4),(4,
1,4),(0.,1.),(0.0610870649866804,0.309114526274187,0.639817807990861),
 .UNSPECIFIED.);
#86=B_SPLINE_SURFACE_WITH_KNOTS('',3,3,((#33827,#33828,#33829,#33830,#33831,
#33832,#33833,#33834,#33835,#33836,#33837,#33838,#33839,#33840,#33841,#33842,
#33843,#33844,#33845,#33846,#33847,#33848,#33849,#33850,#33851,#33852,#33853,
#33854,#33855,#33856,#33857,#33858,#33859,#33860,#33861,#33862,#33863,#33864,
#33865,#33866,#33867,#33868,#33869,#33870,#33871,#33872,#33873,#33874,#33875,
#33876,#33877,#33878,#33879,#33880,#33881,#33882,#33883,#33884,#33885,#33886,
#33887,#33888,#33889),(#33890,#33891,#33892,#33893,#33894,#33895,#33896,
#33897,#33898,#33899,#33900,#33901,#33902,#33903,#33904,#33905,#33906,#33907,
#33908,#33909,#33910,#33911,#33912,#33913,#33914,#33915,#33916,#33917,#33918,
#33919,#33920,#33921,#33922,#33923,#33924,#33925,#33926,#33927,#33928,#33929,
#33930,#33931,#33932,#33933,#33934,#33935,#33936,#33937,#33938,#33939,#33940,
#33941,#33942,#33943,#33944,#33945,#33946,#33947,#33948,#33949,#33950,#33951,
#33952),(#33953,#33954,#33955,#33956,#33957,#33958,#33959,#33960,#33961,
#33962,#33963,#33964,#33965,#33966,#33967,#33968,#33969,#33970,#33971,#33972,
#33973,#33974,#33975,#33976,#33977,#33978,#33979,#33980,#33981,#33982,#33983,
#33984,#33985,#33986,#33987,#33988,#33989,#33990,#33991,#33992,#33993,#33994,
#33995,#33996,#33997,#33998,#33999,#34000,#34001,#34002,#34003,#34004,#34005,
#34006,#34007,#34008,#34009,#34010,#34011,#34012,#34013,#34014,#34015),
(#34016,#34017,#34018,#34019,#34020,#34021,#34022,#34023,#34024,#34025,
#34026,#34027,#34028,#34029,#34030,#34031,#34032,#34033,#34034,#34035,#34036,
#34037,#34038,#34039,#34040,#34041,#34042,#34043,#34044,#34045,#34046,#34047,
#34048,#34049,#34050,#34051,#34052,#34053,#34054,#34055,#34056,#34057,#34058,
#34059,#34060,#34061,#34062,#34063,#34064,#34065,#34066,#34067,#34068,#34069,
#34070,#34071,#34072,#34073,#34074,#34075,#34076,#34077,#34078),(#34079,
#34080,#34081,#34082,#34083,#34084,#34085,#34086,#34087,#34088,#34089,#34090,
#34091,#34092,#34093,#34094,#34095,#34096,#34097,#34098,#34099,#34100,#34101,
#34102,#34103,#34104,#34105,#34106,#34107,#34108,#34109,#34110,#34111,#34112,
#34113,#34114,#34115,#34116,#34117,#34118,#34119,#34120,#34121,#34122,#34123,
#34124,#34125,#34126,#34127,#34128,#34129,#34130,#34131,#34132,#34133,#34134,
#34135,#34136,#34137,#34138,#34139,#34140,#34141),(#34142,#34143,#34144,
#34145,#34146,#34147,#34148,#34149,#34150,#34151,#34152,#34153,#34154,#34155,
#34156,#34157,#34158,#34159,#34160,#34161,#34162,#34163,#34164,#34165,#34166,
#34167,#34168,#34169,#34170,#34171,#34172,#34173,#34174,#34175,#34176,#34177,
#34178,#34179,#34180,#34181,#34182,#34183,#34184,#34185,#34186,#34187,#34188,
#34189,#34190,#34191,#34192,#34193,#34194,#34195,#34196,#34197,#34198,#34199,
#34200,#34201,#34202,#34203,#34204),(#34205,#34206,#34207,#34208,#34209,
#34210,#34211,#34212,#34213,#34214,#34215,#34216,#34217,#34218,#34219,#34220,
#34221,#34222,#34223,#34224,#34225,#34226,#34227,#34228,#34229,#34230,#34231,
#34232,#34233,#34234,#34235,#34236,#34237,#34238,#34239,#34240,#34241,#34242,
#34243,#34244,#34245,#34246,#34247,#34248,#34249,#34250,#34251,#34252,#34253,
#34254,#34255,#34256,#34257,#34258,#34259,#34260,#34261,#34262,#34263,#34264,
#34265,#34266,#34267),(#34268,#34269,#34270,#34271,#34272,#34273,#34274,
#34275,#34276,#34277,#34278,#34279,#34280,#34281,#34282,#34283,#34284,#34285,
#34286,#34287,#34288,#34289,#34290,#34291,#34292,#34293,#34294,#34295,#34296,
#34297,#34298,#34299,#34300,#34301,#34302,#34303,#34304,#34305,#34306,#34307,
#34308,#34309,#34310,#34311,#34312,#34313,#34314,#34315,#34316,#34317,#34318,
#34319,#34320,#34321,#34322,#34323,#34324,#34325,#34326,#34327,#34328,#34329,
#34330),(#34331,#34332,#34333,#34334,#34335,#34336,#34337,#34338,#34339,
#34340,#34341,#34342,#34343,#34344,#34345,#34346,#34347,#34348,#34349,#34350,
#34351,#34352,#34353,#34354,#34355,#34356,#34357,#34358,#34359,#34360,#34361,
#34362,#34363,#34364,#34365,#34366,#34367,#34368,#34369,#34370,#34371,#34372,
#34373,#34374,#34375,#34376,#34377,#34378,#34379,#34380,#34381,#34382,#34383,
#34384,#34385,#34386,#34387,#34388,#34389,#34390,#34391,#34392,#34393),
(#34394,#34395,#34396,#34397,#34398,#34399,#34400,#34401,#34402,#34403,
#34404,#34405,#34406,#34407,#34408,#34409,#34410,#34411,#34412,#34413,#34414,
#34415,#34416,#34417,#34418,#34419,#34420,#34421,#34422,#34423,#34424,#34425,
#34426,#34427,#34428,#34429,#34430,#34431,#34432,#34433,#34434,#34435,#34436,
#34437,#34438,#34439,#34440,#34441,#34442,#34443,#34444,#34445,#34446,#34447,
#34448,#34449,#34450,#34451,#34452,#34453,#34454,#34455,#34456),(#34457,
#34458,#34459,#34460,#34461,#34462,#34463,#34464,#34465,#34466,#34467,#34468,
#34469,#34470,#34471,#34472,#34473,#34474,#34475,#34476,#34477,#34478,#34479,
#34480,#34481,#34482,#34483,#34484,#34485,#34486,#34487,#34488,#34489,#34490,
#34491,#34492,#34493,#34494,#34495,#34496,#34497,#34498,#34499,#34500,#34501,
#34502,#34503,#34504,#34505,#34506,#34507,#34508,#34509,#34510,#34511,#34512,
#34513,#34514,#34515,#34516,#34517,#34518,#34519)),.UNSPECIFIED.,.T.,.F.,
 .F.,(4,1,1,1,1,1,1,1,4),(4,1,1,1,1,1,1,1,1,1,1,1,1,1,1,1,1,1,1,1,1,1,1,
1,1,1,1,1,1,1,1,1,1,1,1,1,1,1,1,1,1,1,1,1,1,1,1,1,1,1,1,1,1,1,1,1,1,1,1,
1,4),(-3.14159265358979,-2.46839422782055,-2.24399475256414,-1.34639685153848,
-0.448798950512828,0.448798950512828,1.34639685153848,2.24399475256414,
3.14159265358979),(0.,0.00892857142857143,0.0178571428571429,0.0357142857142857,
0.0535714285714286,0.0714285714285714,0.0892857142857143,0.107142857142857,
0.125,0.142857142857143,0.154761904761905,0.166666666666667,0.178571428571429,
0.19047619047619,0.202380952380952,0.214285714285714,0.238095238095238,
0.261904761904762,0.273809523809524,0.285714285714286,0.30952380952381,
0.333333333333333,0.357142857142857,0.369047619047619,0.380952380952381,
0.392857142857143,0.404761904761905,0.416666666666667,0.428571428571429,
0.446428571428571,0.464285714285714,0.482142857142857,0.5,0.517857142857143,
0.535714285714286,0.553571428571429,0.571428571428571,0.589285714285714,
0.607142857142857,0.625,0.642857142857143,0.660714285714286,0.678571428571428,
0.696428571428571,0.714285714285714,0.726190476190476,0.738095238095238,
0.761904761904762,0.785714285714286,0.809523809523809,0.833333333333333,
0.857142857142857,0.875,0.892857142857143,0.910714285714286,0.928571428571429,
0.946428571428571,0.964285714285714,0.982142857142857,0.991071428571429,
1.),.UNSPECIFIED.);
#87=B_SPLINE_SURFACE_WITH_KNOTS('',3,3,((#35032,#35033,#35034,#35035,#35036,
#35037,#35038,#35039,#35040,#35041,#35042,#35043,#35044,#35045,#35046,#35047,
#35048,#35049,#35050,#35051,#35052,#35053,#35054,#35055,#35056,#35057,#35058,
#35059,#35060,#35061,#35062),(#35063,#35064,#35065,#35066,#35067,#35068,
#35069,#35070,#35071,#35072,#35073,#35074,#35075,#35076,#35077,#35078,#35079,
#35080,#35081,#35082,#35083,#35084,#35085,#35086,#35087,#35088,#35089,#35090,
#35091,#35092,#35093),(#35094,#35095,#35096,#35097,#35098,#35099,#35100,
#35101,#35102,#35103,#35104,#35105,#35106,#35107,#35108,#35109,#35110,#35111,
#35112,#35113,#35114,#35115,#35116,#35117,#35118,#35119,#35120,#35121,#35122,
#35123,#35124),(#35125,#35126,#35127,#35128,#35129,#35130,#35131,#35132,
#35133,#35134,#35135,#35136,#35137,#35138,#35139,#35140,#35141,#35142,#35143,
#35144,#35145,#35146,#35147,#35148,#35149,#35150,#35151,#35152,#35153,#35154,
#35155)),.UNSPECIFIED.,.F.,.F.,.F.,(4,4),(4,1,1,1,1,1,1,1,1,1,1,1,1,1,1,
1,1,1,1,1,1,1,1,1,1,1,1,1,4),(0.,0.0526254770366344),(8.30815772716268,
9.30733212220219,10.3065065172417,11.3056809122812,12.3048553073207,13.3040297023602,
14.3032040973997,15.3023784924392,16.3015528874787,17.3007272825182,18.2999016775577,
19.2990760725973,20.2982504676368,21.2974248626763,22.2965992577158,23.2957736527553,
24.2949480477948,25.2941224428343,26.2932968378738,27.2924712329133,28.2916456279528,
29.2908200229923,30.2899944180318,31.2891688130713,32.2883432081108,33.2875176031503,
34.2866919981899,35.2858663932294,36.2850407882689),.UNSPECIFIED.);
#88=B_SPLINE_SURFACE_WITH_KNOTS('',3,3,((#35379,#35380,#35381,#35382,#35383,
#35384,#35385,#35386,#35387,#35388,#35389,#35390,#35391,#35392,#35393,#35394,
#35395,#35396,#35397,#35398,#35399,#35400,#35401,#35402,#35403,#35404,#35405,
#35406,#35407,#35408,#35409),(#35410,#35411,#35412,#35413,#35414,#35415,
#35416,#35417,#35418,#35419,#35420,#35421,#35422,#35423,#35424,#35425,#35426,
#35427,#35428,#35429,#35430,#35431,#35432,#35433,#35434,#35435,#35436,#35437,
#35438,#35439,#35440),(#35441,#35442,#35443,#35444,#35445,#35446,#35447,
#35448,#35449,#35450,#35451,#35452,#35453,#35454,#35455,#35456,#35457,#35458,
#35459,#35460,#35461,#35462,#35463,#35464,#35465,#35466,#35467,#35468,#35469,
#35470,#35471),(#35472,#35473,#35474,#35475,#35476,#35477,#35478,#35479,
#35480,#35481,#35482,#35483,#35484,#35485,#35486,#35487,#35488,#35489,#35490,
#35491,#35492,#35493,#35494,#35495,#35496,#35497,#35498,#35499,#35500,#35501,
#35502)),.UNSPECIFIED.,.F.,.F.,.F.,(4,4),(4,1,1,1,1,1,1,1,1,1,1,1,1,1,1,
1,1,1,1,1,1,1,1,1,1,1,1,1,4),(0.,0.0526254770366344),(11.6163931973415,
12.615567592381,13.6147419874205,14.61391638246,15.6130907774995,16.612265172539,
17.6114395675785,18.610613962618,19.6097883576575,20.6089627526971,21.6081371477366,
22.6073115427761,23.6064859378156,24.6056603328551,25.6048347278946,26.6040091229341,
27.6031835179736,28.6023579130131,29.6015323080526,30.6007067030921,31.5998810981316,
32.5990554931711,33.5982298882106,34.5974042832501,35.5965786782897,36.5957530733292,
37.5949274683687,38.5941018634082,39.5932762584477),.UNSPECIFIED.);
#89=B_SPLINE_SURFACE_WITH_KNOTS('',3,3,((#36636,#36637,#36638,#36639,#36640,
#36641,#36642,#36643,#36644,#36645,#36646,#36647,#36648,#36649,#36650,#36651,
#36652,#36653,#36654,#36655,#36656,#36657,#36658,#36659,#36660,#36661,#36662,
#36663,#36664,#36665,#36666,#36667,#36668,#36669,#36670,#36671,#36672,#36673,
#36674,#36675,#36676,#36677,#36678,#36679,#36680,#36681,#36682,#36683,#36684,
#36685,#36686,#36687,#36688,#36689,#36690,#36691,#36692,#36693,#36694,#36695,
#36696,#36697,#36698,#36699,#36700,#36701,#36702,#36703,#36704,#36705,#36706,
#36707,#36708,#36709,#36710,#36711,#36712,#36713,#36714,#36715,#36716,#36717,
#36718,#36719,#36720,#36721,#36722,#36723,#36724,#36725,#36726,#36727,#36728,
#36729,#36730,#36731,#36732),(#36733,#36734,#36735,#36736,#36737,#36738,
#36739,#36740,#36741,#36742,#36743,#36744,#36745,#36746,#36747,#36748,#36749,
#36750,#36751,#36752,#36753,#36754,#36755,#36756,#36757,#36758,#36759,#36760,
#36761,#36762,#36763,#36764,#36765,#36766,#36767,#36768,#36769,#36770,#36771,
#36772,#36773,#36774,#36775,#36776,#36777,#36778,#36779,#36780,#36781,#36782,
#36783,#36784,#36785,#36786,#36787,#36788,#36789,#36790,#36791,#36792,#36793,
#36794,#36795,#36796,#36797,#36798,#36799,#36800,#36801,#36802,#36803,#36804,
#36805,#36806,#36807,#36808,#36809,#36810,#36811,#36812,#36813,#36814,#36815,
#36816,#36817,#36818,#36819,#36820,#36821,#36822,#36823,#36824,#36825,#36826,
#36827,#36828,#36829),(#36830,#36831,#36832,#36833,#36834,#36835,#36836,
#36837,#36838,#36839,#36840,#36841,#36842,#36843,#36844,#36845,#36846,#36847,
#36848,#36849,#36850,#36851,#36852,#36853,#36854,#36855,#36856,#36857,#36858,
#36859,#36860,#36861,#36862,#36863,#36864,#36865,#36866,#36867,#36868,#36869,
#36870,#36871,#36872,#36873,#36874,#36875,#36876,#36877,#36878,#36879,#36880,
#36881,#36882,#36883,#36884,#36885,#36886,#36887,#36888,#36889,#36890,#36891,
#36892,#36893,#36894,#36895,#36896,#36897,#36898,#36899,#36900,#36901,#36902,
#36903,#36904,#36905,#36906,#36907,#36908,#36909,#36910,#36911,#36912,#36913,
#36914,#36915,#36916,#36917,#36918,#36919,#36920,#36921,#36922,#36923,#36924,
#36925,#36926),(#36927,#36928,#36929,#36930,#36931,#36932,#36933,#36934,
#36935,#36936,#36937,#36938,#36939,#36940,#36941,#36942,#36943,#36944,#36945,
#36946,#36947,#36948,#36949,#36950,#36951,#36952,#36953,#36954,#36955,#36956,
#36957,#36958,#36959,#36960,#36961,#36962,#36963,#36964,#36965,#36966,#36967,
#36968,#36969,#36970,#36971,#36972,#36973,#36974,#36975,#36976,#36977,#36978,
#36979,#36980,#36981,#36982,#36983,#36984,#36985,#36986,#36987,#36988,#36989,
#36990,#36991,#36992,#36993,#36994,#36995,#36996,#36997,#36998,#36999,#37000,
#37001,#37002,#37003,#37004,#37005,#37006,#37007,#37008,#37009,#37010,#37011,
#37012,#37013,#37014,#37015,#37016,#37017,#37018,#37019,#37020,#37021,#37022,
#37023)),.UNSPECIFIED.,.F.,.F.,.F.,(4,4),(4,1,1,1,1,1,1,1,1,1,1,1,1,1,1,
1,1,1,1,1,1,1,1,1,1,1,1,1,1,1,1,1,1,1,1,1,1,1,1,1,1,1,1,1,1,1,1,1,1,1,1,
1,1,1,1,1,1,1,1,1,1,1,1,1,1,1,1,1,1,1,1,1,1,1,1,1,1,1,1,1,1,1,1,1,1,1,1,
1,1,1,1,1,1,1,4),(0.,0.0526254770366343),(8.30815772716261,9.30349343669038,
10.2988291462181,11.2941648557459,12.2895005652737,13.2848362748014,14.2801719843292,
15.275507693857,16.2708434033847,17.2661791129125,18.2615148224403,19.256850531968,
20.2521862414958,21.2475219510236,22.2428576605513,23.2381933700791,24.2335290796069,
25.2288647891346,26.2242004986624,27.2195362081902,28.2148719177179,29.2102076272457,
30.2055433367735,31.2008790463012,32.196214755829,33.1915504653568,34.1868861748845,
35.1822218844123,36.1775575939401,37.1728933034678,38.1682290129956,39.1635647225234,
40.1589004320511,41.1542361415789,42.1495718511067,43.1449075606344,44.1402432701622,
45.13557897969,46.1309146892177,47.1262503987455,48.1215861082733,49.116921817801,
50.1122575273288,51.1075932368566,52.1029289463843,53.0982646559121,54.0936003654399,
55.0889360749676,56.0842717844954,57.0796074940232,58.0749432035509,59.0702789130787,
60.0656146226065,61.0609503321342,62.056286041662,63.0516217511898,64.0469574607175,
65.0422931702453,66.0376288797731,67.0329645893008,68.0283002988286,69.0236360083564,
70.0189717178841,71.0143074274119,72.0096431369397,73.0049788464674,74.0003145559952,
74.995650265523,75.9909859750507,76.9863216845785,77.9816573941063,78.976993103634,
79.9723288131618,80.9676645226896,81.9630002322173,82.9583359417451,83.9536716512729,
84.9490073608006,85.9443430703284,86.9396787798562,87.9350144893839,88.9303501989117,
89.9256859084395,90.9210216179672,91.916357327495,92.9116930370228,93.9070287465505,
94.9023644560783,95.8977001656061,96.8930358751338,97.8883715846616,98.8837072941894,
99.8790430037171,100.874378713245,101.869714422773),.UNSPECIFIED.);
#90=B_SPLINE_SURFACE_WITH_KNOTS('',3,3,((#37321,#37322,#37323,#37324,#37325,
#37326,#37327,#37328,#37329,#37330,#37331,#37332,#37333,#37334,#37335,#37336,
#37337,#37338,#37339,#37340,#37341,#37342,#37343,#37344,#37345,#37346,#37347,
#37348,#37349,#37350,#37351,#37352,#37353,#37354,#37355,#37356,#37357,#37358,
#37359,#37360,#37361,#37362,#37363,#37364,#37365,#37366,#37367,#37368,#37369,
#37370,#37371,#37372,#37373,#37374,#37375,#37376,#37377,#37378,#37379,#37380,
#37381,#37382,#37383,#37384,#37385,#37386,#37387,#37388,#37389,#37390,#37391,
#37392,#37393,#37394,#37395,#37396,#37397,#37398,#37399,#37400,#37401,#37402,
#37403,#37404,#37405,#37406,#37407,#37408,#37409,#37410,#37411,#37412,#37413,
#37414,#37415,#37416,#37417),(#37418,#37419,#37420,#37421,#37422,#37423,
#37424,#37425,#37426,#37427,#37428,#37429,#37430,#37431,#37432,#37433,#37434,
#37435,#37436,#37437,#37438,#37439,#37440,#37441,#37442,#37443,#37444,#37445,
#37446,#37447,#37448,#37449,#37450,#37451,#37452,#37453,#37454,#37455,#37456,
#37457,#37458,#37459,#37460,#37461,#37462,#37463,#37464,#37465,#37466,#37467,
#37468,#37469,#37470,#37471,#37472,#37473,#37474,#37475,#37476,#37477,#37478,
#37479,#37480,#37481,#37482,#37483,#37484,#37485,#37486,#37487,#37488,#37489,
#37490,#37491,#37492,#37493,#37494,#37495,#37496,#37497,#37498,#37499,#37500,
#37501,#37502,#37503,#37504,#37505,#37506,#37507,#37508,#37509,#37510,#37511,
#37512,#37513,#37514),(#37515,#37516,#37517,#37518,#37519,#37520,#37521,
#37522,#37523,#37524,#37525,#37526,#37527,#37528,#37529,#37530,#37531,#37532,
#37533,#37534,#37535,#37536,#37537,#37538,#37539,#37540,#37541,#37542,#37543,
#37544,#37545,#37546,#37547,#37548,#37549,#37550,#37551,#37552,#37553,#37554,
#37555,#37556,#37557,#37558,#37559,#37560,#37561,#37562,#37563,#37564,#37565,
#37566,#37567,#37568,#37569,#37570,#37571,#37572,#37573,#37574,#37575,#37576,
#37577,#37578,#37579,#37580,#37581,#37582,#37583,#37584,#37585,#37586,#37587,
#37588,#37589,#37590,#37591,#37592,#37593,#37594,#37595,#37596,#37597,#37598,
#37599,#37600,#37601,#37602,#37603,#37604,#37605,#37606,#37607,#37608,#37609,
#37610,#37611),(#37612,#37613,#37614,#37615,#37616,#37617,#37618,#37619,
#37620,#37621,#37622,#37623,#37624,#37625,#37626,#37627,#37628,#37629,#37630,
#37631,#37632,#37633,#37634,#37635,#37636,#37637,#37638,#37639,#37640,#37641,
#37642,#37643,#37644,#37645,#37646,#37647,#37648,#37649,#37650,#37651,#37652,
#37653,#37654,#37655,#37656,#37657,#37658,#37659,#37660,#37661,#37662,#37663,
#37664,#37665,#37666,#37667,#37668,#37669,#37670,#37671,#37672,#37673,#37674,
#37675,#37676,#37677,#37678,#37679,#37680,#37681,#37682,#37683,#37684,#37685,
#37686,#37687,#37688,#37689,#37690,#37691,#37692,#37693,#37694,#37695,#37696,
#37697,#37698,#37699,#37700,#37701,#37702,#37703,#37704,#37705,#37706,#37707,
#37708)),.UNSPECIFIED.,.F.,.F.,.F.,(4,4),(4,1,1,1,1,1,1,1,1,1,1,1,1,1,1,
1,1,1,1,1,1,1,1,1,1,1,1,1,1,1,1,1,1,1,1,1,1,1,1,1,1,1,1,1,1,1,1,1,1,1,1,
1,1,1,1,1,1,1,1,1,1,1,1,1,1,1,1,1,1,1,1,1,1,1,1,1,1,1,1,1,1,1,1,1,1,1,1,
1,1,1,1,1,1,1,4),(0.,0.0526254770366343),(11.6163931973414,12.6117289068692,
13.6070646163969,14.6024003259247,15.5977360354525,16.5930717449802,17.588407454508,
18.5837431640358,19.5790788735635,20.5744145830913,21.5697502926191,22.5650860021468,
23.5604217116746,24.5557574212024,25.5510931307301,26.5464288402579,27.5417645497857,
28.5371002593134,29.5324359688412,30.527771678369,31.5231073878967,32.5184430974245,
33.5137788069523,34.50911451648,35.5044502260078,36.4997859355356,37.4951216450633,
38.4904573545911,39.4857930641189,40.4811287736466,41.4764644831744,42.4718001927022,
43.4671359022299,44.4624716117577,45.4578073212855,46.4531430308133,47.448478740341,
48.4438144498688,49.4391501593965,50.4344858689243,51.4298215784521,52.4251572879798,
53.4204929975076,54.4158287070354,55.4111644165631,56.4065001260909,57.4018358356187,
58.3971715451464,59.3925072546742,60.387842964202,61.3831786737297,62.3785143832575,
63.3738500927853,64.369185802313,65.3645215118408,66.3598572213686,67.3551929308963,
68.3505286404241,69.3458643499519,70.3412000594796,71.3365357690074,72.3318714785352,
73.3272071880629,74.3225428975907,75.3178786071185,76.3132143166462,77.308550026174,
78.3038857357018,79.2992214452295,80.2945571547573,81.2898928642851,82.2852285738128,
83.2805642833406,84.2758999928684,85.2712357023961,86.2665714119239,87.2619071214517,
88.2572428309794,89.2525785405072,90.247914250035,91.2432499595627,92.2385856690905,
93.2339213786183,94.229257088146,95.2245927976738,96.2199285072016,97.2152642167293,
98.2105999262571,99.2059356357849,100.201271345313,101.19660705484,102.191942764368,
103.187278473896,104.182614183424,105.177949892951),.UNSPECIFIED.);
#91=SHAPE_REPRESENTATION_RELATIONSHIP('SRR','None',#38576,#103);
#92=SHAPE_REPRESENTATION_RELATIONSHIP('SRR','None',#38577,#104);
#93=SHAPE_REPRESENTATION_RELATIONSHIP('SRR','None',#38578,#105);
#94=SHAPE_REPRESENTATION_RELATIONSHIP('SRR','None',#38579,#106);
#95=SHAPE_REPRESENTATION_RELATIONSHIP('SRR','None',#38580,#107);
#96=SHAPE_REPRESENTATION_RELATIONSHIP('SRR','None',#38581,#108);
#97=SHAPE_REPRESENTATION_RELATIONSHIP('SRR','None',#38582,#109);
#98=SHAPE_REPRESENTATION_RELATIONSHIP('SRR','None',#38583,#110);
#99=SHAPE_REPRESENTATION_RELATIONSHIP('SRR','None',#38584,#111);
#100=SHAPE_REPRESENTATION_RELATIONSHIP('SRR','None',#38585,#112);
#101=SHAPE_REPRESENTATION_RELATIONSHIP('SRR','None',#38586,#113);
#102=SHAPE_REPRESENTATION_RELATIONSHIP('SRR','None',#38587,#114);
#103=ADVANCED_BREP_SHAPE_REPRESENTATION('',(#127),#38516);
#104=ADVANCED_BREP_SHAPE_REPRESENTATION('',(#128),#38517);
#105=ADVANCED_BREP_SHAPE_REPRESENTATION('',(#129),#38518);
#106=ADVANCED_BREP_SHAPE_REPRESENTATION('',(#130),#38519);
#107=ADVANCED_BREP_SHAPE_REPRESENTATION('',(#131),#38520);
#108=ADVANCED_BREP_SHAPE_REPRESENTATION('',(#132),#38521);
#109=ADVANCED_BREP_SHAPE_REPRESENTATION('',(#133),#38522);
#110=ADVANCED_BREP_SHAPE_REPRESENTATION('',(#134),#38523);
#111=ADVANCED_BREP_SHAPE_REPRESENTATION('',(#135),#38524);
#112=ADVANCED_BREP_SHAPE_REPRESENTATION('',(#136),#38525);
#113=ADVANCED_BREP_SHAPE_REPRESENTATION('',(#137),#38526);
#114=ADVANCED_BREP_SHAPE_REPRESENTATION('',(#138),#38527);
#115=STYLED_ITEM('',(#38685),#127);
#116=STYLED_ITEM('',(#38720),#128);
#117=STYLED_ITEM('',(#38692),#129);
#118=STYLED_ITEM('',(#38692),#130);
#119=STYLED_ITEM('',(#38692),#131);
#120=STYLED_ITEM('',(#38713),#132);
#121=STYLED_ITEM('',(#38713),#133);
#122=STYLED_ITEM('',(#38713),#134);
#123=STYLED_ITEM('',(#38720),#135);
#124=STYLED_ITEM('',(#38706),#136);
#125=STYLED_ITEM('',(#38713),#137);
#126=STYLED_ITEM('',(#38713),#138);
#127=MANIFOLD_SOLID_BREP('Body1',#17072);
#128=MANIFOLD_SOLID_BREP('Body1',#17073);
#129=MANIFOLD_SOLID_BREP('Body1',#17074);
#130=MANIFOLD_SOLID_BREP('Body1',#17075);
#131=MANIFOLD_SOLID_BREP('Body1',#17076);
#132=MANIFOLD_SOLID_BREP('Body1',#17077);
#133=MANIFOLD_SOLID_BREP('Body1',#17078);
#134=MANIFOLD_SOLID_BREP('Body1',#17079);
#135=MANIFOLD_SOLID_BREP('Body1',#17080);
#136=MANIFOLD_SOLID_BREP('Body1',#17081);
#137=MANIFOLD_SOLID_BREP('Body1',#17082);
#138=MANIFOLD_SOLID_BREP('Body1',#17083);
#139=CYLINDRICAL_SURFACE('',#17258,6.);
#140=CYLINDRICAL_SURFACE('',#17281,2.55);
#141=CYLINDRICAL_SURFACE('',#17296,48.);
#142=CYLINDRICAL_SURFACE('',#17299,11.);
#143=CYLINDRICAL_SURFACE('',#17308,2.55);
#144=CYLINDRICAL_SURFACE('',#17313,2.05);
#145=CYLINDRICAL_SURFACE('',#17314,5.);
#146=CYLINDRICAL_SURFACE('',#17325,53.5);
#147=CYLINDRICAL_SURFACE('',#17331,53.5);
#148=CYLINDRICAL_SURFACE('',#17337,0.700000000000003);
#149=CYLINDRICAL_SURFACE('',#17344,0.700000000000003);
#150=CYLINDRICAL_SURFACE('',#17347,0.700000000000003);
#151=CYLINDRICAL_SURFACE('',#17356,0.700000000000003);
#152=CYLINDRICAL_SURFACE('',#17361,0.700000000000003);
#153=CYLINDRICAL_SURFACE('',#17368,53.5);
#154=CYLINDRICAL_SURFACE('',#17377,53.5);
#155=CYLINDRICAL_SURFACE('',#17384,53.5);
#156=CYLINDRICAL_SURFACE('',#17391,53.5);
#157=CYLINDRICAL_SURFACE('',#17398,53.5);
#158=CYLINDRICAL_SURFACE('',#17405,53.5);
#159=CYLINDRICAL_SURFACE('',#17412,53.5);
#160=CYLINDRICAL_SURFACE('',#17419,53.5);
#161=CYLINDRICAL_SURFACE('',#17426,53.5);
#162=CYLINDRICAL_SURFACE('',#17602,0.700000000000003);
#163=CYLINDRICAL_SURFACE('',#17608,0.700000000000003);
#164=CYLINDRICAL_SURFACE('',#17614,0.700000000000003);
#165=CYLINDRICAL_SURFACE('',#17620,0.700000000000003);
#166=CYLINDRICAL_SURFACE('',#17623,53.5);
#167=CYLINDRICAL_SURFACE('',#17631,53.5);
#168=CYLINDRICAL_SURFACE('',#17637,53.5);
#169=CYLINDRICAL_SURFACE('',#17643,53.5);
#170=CYLINDRICAL_SURFACE('',#17649,53.5);
#171=CYLINDRICAL_SURFACE('',#17655,53.5);
#172=CYLINDRICAL_SURFACE('',#17661,53.5);
#173=CYLINDRICAL_SURFACE('',#17670,53.5);
#174=CYLINDRICAL_SURFACE('',#17672,53.5);
#175=CYLINDRICAL_SURFACE('',#17674,53.5);
#176=CYLINDRICAL_SURFACE('',#17687,0.700000000000003);
#177=CYLINDRICAL_SURFACE('',#17689,0.700000000000003);
#178=CYLINDRICAL_SURFACE('',#17691,0.700000000000003);
#179=CYLINDRICAL_SURFACE('',#17693,0.700000000000003);
#180=CYLINDRICAL_SURFACE('',#17695,0.700000000000003);
#181=CYLINDRICAL_SURFACE('',#17697,0.700000000000003);
#182=CYLINDRICAL_SURFACE('',#17702,0.700000000000003);
#183=CYLINDRICAL_SURFACE('',#17710,0.700000000000003);
#184=CYLINDRICAL_SURFACE('',#17716,0.700000000000003);
#185=CYLINDRICAL_SURFACE('',#17722,0.700000000000003);
#186=CYLINDRICAL_SURFACE('',#17725,53.5);
#187=CYLINDRICAL_SURFACE('',#17733,53.5);
#188=CYLINDRICAL_SURFACE('',#17739,53.5);
#189=CYLINDRICAL_SURFACE('',#17745,53.5);
#190=CYLINDRICAL_SURFACE('',#17751,53.5);
#191=CYLINDRICAL_SURFACE('',#17757,53.5);
#192=CYLINDRICAL_SURFACE('',#17766,53.5);
#193=CYLINDRICAL_SURFACE('',#17768,53.5);
#194=CYLINDRICAL_SURFACE('',#17770,53.5);
#195=CYLINDRICAL_SURFACE('',#17772,53.5);
#196=CYLINDRICAL_SURFACE('',#17783,0.700000000000003);
#197=CYLINDRICAL_SURFACE('',#17785,0.700000000000003);
#198=CYLINDRICAL_SURFACE('',#17787,0.700000000000003);
#199=CYLINDRICAL_SURFACE('',#17789,0.700000000000003);
#200=CYLINDRICAL_SURFACE('',#17791,0.700000000000003);
#201=CYLINDRICAL_SURFACE('',#17796,0.700000000000003);
#202=CYLINDRICAL_SURFACE('',#17802,0.700000000000003);
#203=CYLINDRICAL_SURFACE('',#17808,0.700000000000003);
#204=CYLINDRICAL_SURFACE('',#17814,0.700000000000003);
#205=CYLINDRICAL_SURFACE('',#17820,0.700000000000003);
#206=CYLINDRICAL_SURFACE('',#17823,53.5);
#207=CYLINDRICAL_SURFACE('',#17831,53.5);
#208=CYLINDRICAL_SURFACE('',#17837,53.5);
#209=CYLINDRICAL_SURFACE('',#17843,53.5);
#210=CYLINDRICAL_SURFACE('',#17849,53.5);
#211=CYLINDRICAL_SURFACE('',#17862,53.5);
#212=CYLINDRICAL_SURFACE('',#17864,53.5);
#213=CYLINDRICAL_SURFACE('',#17866,53.5);
#214=CYLINDRICAL_SURFACE('',#17868,53.5);
#215=CYLINDRICAL_SURFACE('',#17870,53.5);
#216=CYLINDRICAL_SURFACE('',#17879,0.700000000000003);
#217=CYLINDRICAL_SURFACE('',#17881,0.700000000000003);
#218=CYLINDRICAL_SURFACE('',#17883,0.700000000000003);
#219=CYLINDRICAL_SURFACE('',#17885,0.700000000000003);
#220=CYLINDRICAL_SURFACE('',#17890,0.700000000000003);
#221=CYLINDRICAL_SURFACE('',#17898,0.700000000000003);
#222=CYLINDRICAL_SURFACE('',#17904,0.700000000000003);
#223=CYLINDRICAL_SURFACE('',#17910,0.700000000000003);
#224=CYLINDRICAL_SURFACE('',#17916,0.700000000000003);
#225=CYLINDRICAL_SURFACE('',#17922,0.700000000000003);
#226=CYLINDRICAL_SURFACE('',#17925,53.5);
#227=CYLINDRICAL_SURFACE('',#17933,53.5);
#228=CYLINDRICAL_SURFACE('',#17939,53.5);
#229=CYLINDRICAL_SURFACE('',#17945,53.5);
#230=CYLINDRICAL_SURFACE('',#17958,53.5);
#231=CYLINDRICAL_SURFACE('',#17960,53.5);
#232=CYLINDRICAL_SURFACE('',#17962,53.5);
#233=CYLINDRICAL_SURFACE('',#17964,53.5);
#234=CYLINDRICAL_SURFACE('',#17966,53.5);
#235=CYLINDRICAL_SURFACE('',#17968,53.5);
#236=CYLINDRICAL_SURFACE('',#17975,0.700000000000003);
#237=CYLINDRICAL_SURFACE('',#17977,0.700000000000003);
#238=CYLINDRICAL_SURFACE('',#17979,0.700000000000003);
#239=CYLINDRICAL_SURFACE('',#17984,0.700000000000003);
#240=CYLINDRICAL_SURFACE('',#17990,0.700000000000003);
#241=CYLINDRICAL_SURFACE('',#17996,0.700000000000003);
#242=CYLINDRICAL_SURFACE('',#18002,0.700000000000003);
#243=CYLINDRICAL_SURFACE('',#18008,0.700000000000003);
#244=CYLINDRICAL_SURFACE('',#18014,0.700000000000003);
#245=CYLINDRICAL_SURFACE('',#18020,0.700000000000003);
#246=CYLINDRICAL_SURFACE('',#18023,53.5);
#247=CYLINDRICAL_SURFACE('',#18031,53.5);
#248=CYLINDRICAL_SURFACE('',#18037,53.5);
#249=CYLINDRICAL_SURFACE('',#18054,53.5);
#250=CYLINDRICAL_SURFACE('',#18056,53.5);
#251=CYLINDRICAL_SURFACE('',#18058,53.5);
#252=CYLINDRICAL_SURFACE('',#18060,53.5);
#253=CYLINDRICAL_SURFACE('',#18062,53.5);
#254=CYLINDRICAL_SURFACE('',#18064,53.5);
#255=CYLINDRICAL_SURFACE('',#18066,53.5);
#256=CYLINDRICAL_SURFACE('',#18071,0.700000000000003);
#257=CYLINDRICAL_SURFACE('',#18073,0.700000000000003);
#258=CYLINDRICAL_SURFACE('',#18078,0.700000000000003);
#259=CYLINDRICAL_SURFACE('',#18084,0.700000000000003);
#260=CYLINDRICAL_SURFACE('',#18090,0.700000000000003);
#261=CYLINDRICAL_SURFACE('',#18096,0.700000000000003);
#262=CYLINDRICAL_SURFACE('',#18102,0.700000000000003);
#263=CYLINDRICAL_SURFACE('',#18108,0.700000000000003);
#264=CYLINDRICAL_SURFACE('',#18114,0.700000000000003);
#265=CYLINDRICAL_SURFACE('',#18120,0.700000000000003);
#266=CYLINDRICAL_SURFACE('',#18123,53.5);
#267=CYLINDRICAL_SURFACE('',#18131,53.5);
#268=CYLINDRICAL_SURFACE('',#18150,53.5);
#269=CYLINDRICAL_SURFACE('',#18152,53.5);
#270=CYLINDRICAL_SURFACE('',#18154,53.5);
#271=CYLINDRICAL_SURFACE('',#18156,53.5);
#272=CYLINDRICAL_SURFACE('',#18158,53.5);
#273=CYLINDRICAL_SURFACE('',#18160,53.5);
#274=CYLINDRICAL_SURFACE('',#18162,53.5);
#275=CYLINDRICAL_SURFACE('',#18164,53.5);
#276=CYLINDRICAL_SURFACE('',#18167,0.700000000000003);
#277=CYLINDRICAL_SURFACE('',#18172,53.5);
#278=CYLINDRICAL_SURFACE('',#18178,53.5);
#279=CYLINDRICAL_SURFACE('',#18184,53.5);
#280=CYLINDRICAL_SURFACE('',#18190,53.5);
#281=CYLINDRICAL_SURFACE('',#18196,53.5);
#282=CYLINDRICAL_SURFACE('',#18202,53.5);
#283=CYLINDRICAL_SURFACE('',#18208,53.5);
#284=CYLINDRICAL_SURFACE('',#18214,53.5);
#285=CYLINDRICAL_SURFACE('',#18220,53.5);
#286=CYLINDRICAL_SURFACE('',#18223,0.700000000000003);
#287=CYLINDRICAL_SURFACE('',#18244,0.700000000000003);
#288=CYLINDRICAL_SURFACE('',#18246,0.700000000000003);
#289=CYLINDRICAL_SURFACE('',#18248,0.700000000000003);
#290=CYLINDRICAL_SURFACE('',#18250,0.700000000000003);
#291=CYLINDRICAL_SURFACE('',#18252,0.700000000000003);
#292=CYLINDRICAL_SURFACE('',#18254,0.700000000000003);
#293=CYLINDRICAL_SURFACE('',#18256,0.700000000000003);
#294=CYLINDRICAL_SURFACE('',#18258,0.700000000000003);
#295=CYLINDRICAL_SURFACE('',#18262,49.5);
#296=CYLINDRICAL_SURFACE('',#18281,0.700000000000003);
#297=CYLINDRICAL_SURFACE('',#18283,0.700000000000003);
#298=CYLINDRICAL_SURFACE('',#18285,0.700000000000003);
#299=CYLINDRICAL_SURFACE('',#18287,0.700000000000003);
#300=CYLINDRICAL_SURFACE('',#18289,0.700000000000003);
#301=CYLINDRICAL_SURFACE('',#18291,0.700000000000003);
#302=CYLINDRICAL_SURFACE('',#18293,0.700000000000003);
#303=CYLINDRICAL_SURFACE('',#18295,0.700000000000003);
#304=CYLINDRICAL_SURFACE('',#18297,0.700000000000003);
#305=CYLINDRICAL_SURFACE('',#18300,0.700000000000003);
#306=CYLINDRICAL_SURFACE('',#18306,0.700000000000003);
#307=CYLINDRICAL_SURFACE('',#18312,0.700000000000003);
#308=CYLINDRICAL_SURFACE('',#18318,0.700000000000003);
#309=CYLINDRICAL_SURFACE('',#18324,0.700000000000003);
#310=CYLINDRICAL_SURFACE('',#18330,0.700000000000003);
#311=CYLINDRICAL_SURFACE('',#18453,12.5);
#312=CYLINDRICAL_SURFACE('',#18457,12.5);
#313=CYLINDRICAL_SURFACE('',#18461,12.5);
#314=CYLINDRICAL_SURFACE('',#18465,12.5);
#315=CYLINDRICAL_SURFACE('',#18469,12.5);
#316=CYLINDRICAL_SURFACE('',#18473,50.5);
#317=CYLINDRICAL_SURFACE('',#18474,53.5);
#318=CYLINDRICAL_SURFACE('',#18475,53.5);
#319=CYLINDRICAL_SURFACE('',#18476,53.5);
#320=CYLINDRICAL_SURFACE('',#18477,53.5);
#321=CYLINDRICAL_SURFACE('',#18478,53.5);
#322=CYLINDRICAL_SURFACE('',#18479,53.5);
#323=CYLINDRICAL_SURFACE('',#18480,53.5);
#324=CYLINDRICAL_SURFACE('',#18481,53.5);
#325=CYLINDRICAL_SURFACE('',#18482,53.5);
#326=CYLINDRICAL_SURFACE('',#18483,53.5);
#327=CYLINDRICAL_SURFACE('',#18490,0.700000000000003);
#328=CYLINDRICAL_SURFACE('',#18502,0.700000000000003);
#329=CYLINDRICAL_SURFACE('',#18514,0.700000000000003);
#330=CYLINDRICAL_SURFACE('',#18558,0.700000000000003);
#331=CYLINDRICAL_SURFACE('',#18568,0.700000000000003);
#332=CYLINDRICAL_SURFACE('',#18580,0.700000000000003);
#333=CYLINDRICAL_SURFACE('',#18596,5.025);
#334=CYLINDRICAL_SURFACE('',#18600,9.64155);
#335=CYLINDRICAL_SURFACE('',#18602,9.64155);
#336=CYLINDRICAL_SURFACE('',#18603,9.64155);
#337=CYLINDRICAL_SURFACE('',#18604,9.64155);
#338=CYLINDRICAL_SURFACE('',#18605,9.64155);
#339=CYLINDRICAL_SURFACE('',#18606,9.64155);
#340=CYLINDRICAL_SURFACE('',#18607,9.64155);
#341=CYLINDRICAL_SURFACE('',#18608,9.64155);
#342=CYLINDRICAL_SURFACE('',#18609,9.64155);
#343=CYLINDRICAL_SURFACE('',#18610,9.64155);
#344=CYLINDRICAL_SURFACE('',#18611,9.64155);
#345=CYLINDRICAL_SURFACE('',#18612,9.64155);
#346=CYLINDRICAL_SURFACE('',#18614,10.06205);
#347=CYLINDRICAL_SURFACE('',#18616,10.06205);
#348=CYLINDRICAL_SURFACE('',#18617,10.06205);
#349=CYLINDRICAL_SURFACE('',#18618,10.06205);
#350=CYLINDRICAL_SURFACE('',#18619,10.06205);
#351=CYLINDRICAL_SURFACE('',#18620,10.06205);
#352=CYLINDRICAL_SURFACE('',#18621,10.06205);
#353=CYLINDRICAL_SURFACE('',#18622,10.06205);
#354=CYLINDRICAL_SURFACE('',#18623,10.06205);
#355=CYLINDRICAL_SURFACE('',#18624,10.06205);
#356=CYLINDRICAL_SURFACE('',#18625,10.06205);
#357=CYLINDRICAL_SURFACE('',#18626,10.06205);
#358=CYLINDRICAL_SURFACE('',#18628,10.06205);
#359=CYLINDRICAL_SURFACE('',#18631,9.64155);
#360=CYLINDRICAL_SURFACE('',#18632,12.5);
#361=CYLINDRICAL_SURFACE('',#18636,13.5);
#362=CYLINDRICAL_SURFACE('',#18642,2.942);
#363=CYLINDRICAL_SURFACE('',#18644,2.942);
#364=CYLINDRICAL_SURFACE('',#18645,2.942);
#365=CYLINDRICAL_SURFACE('',#18646,2.942);
#366=CYLINDRICAL_SURFACE('',#18647,2.942);
#367=CYLINDRICAL_SURFACE('',#18648,2.942);
#368=CYLINDRICAL_SURFACE('',#18649,2.37175);
#369=CYLINDRICAL_SURFACE('',#18651,2.37175);
#370=CYLINDRICAL_SURFACE('',#18652,2.37175);
#371=CYLINDRICAL_SURFACE('',#18653,2.37175);
#372=CYLINDRICAL_SURFACE('',#18654,2.37175);
#373=CYLINDRICAL_SURFACE('',#18655,2.37175);
#374=CYLINDRICAL_SURFACE('',#18659,2.37175);
#375=CYLINDRICAL_SURFACE('',#18661,2.942);
#376=CYLINDRICAL_SURFACE('',#18667,5.);
#377=CYLINDRICAL_SURFACE('',#18686,5.6);
#378=CYLINDRICAL_SURFACE('',#18688,5.);
#379=CYLINDRICAL_SURFACE('',#18691,8.2);
#380=CYLINDRICAL_SURFACE('',#18696,11.);
#381=CYLINDRICAL_SURFACE('',#18700,5.25);
#382=CYLINDRICAL_SURFACE('',#18705,12.);
#383=CYLINDRICAL_SURFACE('',#18713,6.);
#384=CYLINDRICAL_SURFACE('',#18717,3.2);
#385=CYLINDRICAL_SURFACE('',#18726,3.05);
#386=CYLINDRICAL_SURFACE('',#18775,2.4505);
#387=CYLINDRICAL_SURFACE('',#18777,2.4505);
#388=CYLINDRICAL_SURFACE('',#18778,2.4505);
#389=CYLINDRICAL_SURFACE('',#18779,2.4505);
#390=CYLINDRICAL_SURFACE('',#18780,1.99475);
#391=CYLINDRICAL_SURFACE('',#18782,1.99475);
#392=CYLINDRICAL_SURFACE('',#18783,1.99475);
#393=CYLINDRICAL_SURFACE('',#18784,1.99475);
#394=CYLINDRICAL_SURFACE('',#18792,1.99475);
#395=CYLINDRICAL_SURFACE('',#18803,2.4505);
#396=CYLINDRICAL_SURFACE('',#18809,2.4505);
#397=CYLINDRICAL_SURFACE('',#18811,2.4505);
#398=CYLINDRICAL_SURFACE('',#18812,2.4505);
#399=CYLINDRICAL_SURFACE('',#18813,2.4505);
#400=CYLINDRICAL_SURFACE('',#18814,2.4505);
#401=CYLINDRICAL_SURFACE('',#18815,2.4505);
#402=CYLINDRICAL_SURFACE('',#18816,2.4505);
#403=CYLINDRICAL_SURFACE('',#18817,2.4505);
#404=CYLINDRICAL_SURFACE('',#18818,2.4505);
#405=CYLINDRICAL_SURFACE('',#18819,2.4505);
#406=CYLINDRICAL_SURFACE('',#18820,2.4505);
#407=CYLINDRICAL_SURFACE('',#18821,2.4505);
#408=CYLINDRICAL_SURFACE('',#18822,2.4505);
#409=CYLINDRICAL_SURFACE('',#18823,2.4505);
#410=CYLINDRICAL_SURFACE('',#18824,2.4505);
#411=CYLINDRICAL_SURFACE('',#18825,1.99475);
#412=CYLINDRICAL_SURFACE('',#18827,1.99475);
#413=CYLINDRICAL_SURFACE('',#18828,1.99475);
#414=CYLINDRICAL_SURFACE('',#18829,1.99475);
#415=CYLINDRICAL_SURFACE('',#18830,1.99475);
#416=CYLINDRICAL_SURFACE('',#18831,1.99475);
#417=CYLINDRICAL_SURFACE('',#18832,1.99475);
#418=CYLINDRICAL_SURFACE('',#18833,1.99475);
#419=CYLINDRICAL_SURFACE('',#18834,1.99475);
#420=CYLINDRICAL_SURFACE('',#18835,1.99475);
#421=CYLINDRICAL_SURFACE('',#18836,1.99475);
#422=CYLINDRICAL_SURFACE('',#18837,1.99475);
#423=CYLINDRICAL_SURFACE('',#18838,1.99475);
#424=CYLINDRICAL_SURFACE('',#18839,1.99475);
#425=CYLINDRICAL_SURFACE('',#18844,1.99475);
#426=CYLINDRICAL_SURFACE('',#18849,5.);
#427=CYLINDRICAL_SURFACE('',#19001,2.4505);
#428=B_SPLINE_CURVE_WITH_KNOTS('',3,(#23818,#23819,#23820,#23821,#23822,
#23823),.UNSPECIFIED.,.F.,.F.,(4,2,4),(2.30648016522772,2.36442361206073,
2.39897284114794),.UNSPECIFIED.);
#429=B_SPLINE_CURVE_WITH_KNOTS('',3,(#23838,#23839,#23840,#23841,#23842,
#23843),.UNSPECIFIED.,.F.,.F.,(4,2,4),(1.51323695998699,1.54778618907421,
1.60572963590723),.UNSPECIFIED.);
#430=B_SPLINE_CURVE_WITH_KNOTS('',3,(#23844,#23845,#23846,#23847,#23848,
#23849,#23850,#23851,#23852,#23853,#23854,#23855,#23856,#23857,#23858,#23859,
#23860,#23861,#23862,#23863,#23864,#23865,#23866,#23867,#23868,#23869,#23870,
#23871,#23872,#23873,#23874),.UNSPECIFIED.,.F.,.F.,(4,2,2,3,2,2,2,2,2,2,
2,2,2,2,4),(-0.489813721019733,-0.452534469426352,-0.226267234713176,0.,
0.226267234713176,0.452534469426352,0.678799813883625,0.905065158340898,
1.13133050279817,1.35759584725544,1.58386308196862,1.8101303166818,2.03639755139497,
2.26266478610815,2.29994403770815),.UNSPECIFIED.);
#431=B_SPLINE_CURVE_WITH_KNOTS('',3,(#24013,#24014,#24015,#24016),
 .UNSPECIFIED.,.F.,.F.,(4,4),(0.165217092335985,0.177184346430037),
 .UNSPECIFIED.);
#432=B_SPLINE_CURVE_WITH_KNOTS('',3,(#24020,#24021,#24022,#24023),
 .UNSPECIFIED.,.F.,.F.,(4,4),(0.,0.0446132763744268),.UNSPECIFIED.);
#433=B_SPLINE_CURVE_WITH_KNOTS('',3,(#24050,#24051,#24052,#24053),
 .UNSPECIFIED.,.F.,.F.,(4,4),(0.0319696744346156,0.0766821311551608),
 .UNSPECIFIED.);
#434=B_SPLINE_CURVE_WITH_KNOTS('',3,(#24057,#24058,#24059,#24060),
 .UNSPECIFIED.,.F.,.F.,(4,4),(0.077355308281931,0.0893225623759921),
 .UNSPECIFIED.);
#435=B_SPLINE_CURVE_WITH_KNOTS('',3,(#24072,#24073,#24074,#24075),
 .UNSPECIFIED.,.F.,.F.,(4,4),(0.165217092335986,0.177184346430046),
 .UNSPECIFIED.);
#436=B_SPLINE_CURVE_WITH_KNOTS('',3,(#24102,#24103,#24104,#24105),
 .UNSPECIFIED.,.F.,.F.,(4,4),(0.0319696744346149,0.0766821311551634),
 .UNSPECIFIED.);
#437=B_SPLINE_CURVE_WITH_KNOTS('',3,(#24108,#24109,#24110,#24111),
 .UNSPECIFIED.,.F.,.F.,(4,4),(0.0319696744346139,0.0766821311551655),
 .UNSPECIFIED.);
#438=B_SPLINE_CURVE_WITH_KNOTS('',3,(#24136,#24137,#24138,#24139),
 .UNSPECIFIED.,.F.,.F.,(4,4),(0.031969674434604,0.0766821311551636),
 .UNSPECIFIED.);
#439=B_SPLINE_CURVE_WITH_KNOTS('',3,(#24164,#24165,#24166,#24167),
 .UNSPECIFIED.,.F.,.F.,(4,4),(0.0319696744346154,0.0766821311551577),
 .UNSPECIFIED.);
#440=B_SPLINE_CURVE_WITH_KNOTS('',3,(#24170,#24171,#24172,#24173),
 .UNSPECIFIED.,.F.,.F.,(4,4),(0.0319696744346157,0.0766821311551629),
 .UNSPECIFIED.);
#441=B_SPLINE_CURVE_WITH_KNOTS('',3,(#24207,#24208,#24209,#24210),
 .UNSPECIFIED.,.F.,.F.,(4,4),(0.0773553082819434,0.089322562375993),
 .UNSPECIFIED.);
#442=B_SPLINE_CURVE_WITH_KNOTS('',3,(#24214,#24215,#24216,#24217),
 .UNSPECIFIED.,.F.,.F.,(4,4),(-0.177184216772292,-0.165217092335991),
 .UNSPECIFIED.);
#443=B_SPLINE_CURVE_WITH_KNOTS('',3,(#24225,#24226,#24227,#24228),
 .UNSPECIFIED.,.F.,.F.,(4,4),(0.,0.0964441447221119),.UNSPECIFIED.);
#444=B_SPLINE_CURVE_WITH_KNOTS('',3,(#24230,#24231,#24232,#24233),
 .UNSPECIFIED.,.F.,.F.,(4,4),(0.336279561120239,0.348246685406907),
 .UNSPECIFIED.);
#445=B_SPLINE_CURVE_WITH_KNOTS('',3,(#24258,#24259,#24260,#24261),
 .UNSPECIFIED.,.F.,.F.,(4,4),(0.0319696744346043,0.0766821311551631),
 .UNSPECIFIED.);
#446=B_SPLINE_CURVE_WITH_KNOTS('',3,(#24265,#24266,#24267,#24268),
 .UNSPECIFIED.,.F.,.F.,(4,4),(-0.0893225623759883,-0.0773554379396765),
 .UNSPECIFIED.);
#447=B_SPLINE_CURVE_WITH_KNOTS('',3,(#24269,#24270,#24271,#24272),
 .UNSPECIFIED.,.F.,.F.,(4,4),(0.,0.0964441447217045),.UNSPECIFIED.);
#448=B_SPLINE_CURVE_WITH_KNOTS('',3,(#24296,#24297,#24298,#24299),
 .UNSPECIFIED.,.F.,.F.,(4,4),(0.0319696744346058,0.0766821311551602),
 .UNSPECIFIED.);
#449=B_SPLINE_CURVE_WITH_KNOTS('',3,(#24302,#24303,#24304,#24305),
 .UNSPECIFIED.,.F.,.F.,(4,4),(0.0319696744346046,0.0766821311551621),
 .UNSPECIFIED.);
#450=B_SPLINE_CURVE_WITH_KNOTS('',3,(#24341,#24342,#24343,#24344),
 .UNSPECIFIED.,.F.,.F.,(4,4),(0.0319696744346149,0.0766821311551593),
 .UNSPECIFIED.);
#451=B_SPLINE_CURVE_WITH_KNOTS('',3,(#24347,#24348,#24349,#24350),
 .UNSPECIFIED.,.F.,.F.,(4,4),(0.0319696744346029,0.0766821311551658),
 .UNSPECIFIED.);
#452=B_SPLINE_CURVE_WITH_KNOTS('',3,(#24386,#24387,#24388,#24389),
 .UNSPECIFIED.,.F.,.F.,(4,4),(0.0319696744346075,0.0766821311551552),
 .UNSPECIFIED.);
#453=B_SPLINE_CURVE_WITH_KNOTS('',3,(#24392,#24393,#24394,#24395),
 .UNSPECIFIED.,.F.,.F.,(4,4),(0.0319696744346153,0.0766821311551614),
 .UNSPECIFIED.);
#454=B_SPLINE_CURVE_WITH_KNOTS('',3,(#24431,#24432,#24433,#24434),
 .UNSPECIFIED.,.F.,.F.,(4,4),(0.0319696744346164,0.0766821311551606),
 .UNSPECIFIED.);
#455=B_SPLINE_CURVE_WITH_KNOTS('',3,(#24437,#24438,#24439,#24440),
 .UNSPECIFIED.,.F.,.F.,(4,4),(0.0319696744346151,0.0766821311551609),
 .UNSPECIFIED.);
#456=B_SPLINE_CURVE_WITH_KNOTS('',3,(#24476,#24477,#24478,#24479),
 .UNSPECIFIED.,.F.,.F.,(4,4),(0.0319696744346051,0.076682131155159),
 .UNSPECIFIED.);
#457=B_SPLINE_CURVE_WITH_KNOTS('',3,(#24482,#24483,#24484,#24485),
 .UNSPECIFIED.,.F.,.F.,(4,4),(0.0319696744346129,0.0766821311551604),
 .UNSPECIFIED.);
#458=B_SPLINE_CURVE_WITH_KNOTS('',3,(#24521,#24522,#24523,#24524),
 .UNSPECIFIED.,.F.,.F.,(4,4),(0.0319696744346068,0.0766821311551503),
 .UNSPECIFIED.);
#459=B_SPLINE_CURVE_WITH_KNOTS('',3,(#24527,#24528,#24529,#24530),
 .UNSPECIFIED.,.F.,.F.,(4,4),(0.031969674434606,0.0766821311551618),
 .UNSPECIFIED.);
#460=B_SPLINE_CURVE_WITH_KNOTS('',3,(#24566,#24567,#24568,#24569),
 .UNSPECIFIED.,.F.,.F.,(4,4),(0.0319696744346057,0.0766821311551617),
 .UNSPECIFIED.);
#461=B_SPLINE_CURVE_WITH_KNOTS('',3,(#24572,#24573,#24574,#24575),
 .UNSPECIFIED.,.F.,.F.,(4,4),(0.0319696744346062,0.0766821311551594),
 .UNSPECIFIED.);
#462=B_SPLINE_CURVE_WITH_KNOTS('',3,(#24611,#24612,#24613,#24614),
 .UNSPECIFIED.,.F.,.F.,(4,4),(0.0319696744346062,0.0766821311551613),
 .UNSPECIFIED.);
#463=B_SPLINE_CURVE_WITH_KNOTS('',3,(#24617,#24618,#24619,#24620),
 .UNSPECIFIED.,.F.,.F.,(4,4),(0.0319696744346139,0.0766821311551679),
 .UNSPECIFIED.);
#464=B_SPLINE_CURVE_WITH_KNOTS('',3,(#24641,#24642,#24643,#24644,#24645,
#24646),.UNSPECIFIED.,.F.,.F.,(4,2,4),(1.36037627907923,1.38960835652673,
1.40296484627234),.UNSPECIFIED.);
#465=B_SPLINE_CURVE_WITH_KNOTS('',3,(#24662,#24663,#24664,#24665),
 .UNSPECIFIED.,.F.,.F.,(4,4),(0.16521709233599,0.177184216772299),
 .UNSPECIFIED.);
#466=B_SPLINE_CURVE_WITH_KNOTS('',3,(#24983,#24984,#24985,#24986),
 .UNSPECIFIED.,.F.,.F.,(4,4),(-0.0893225623759853,-0.0773554379396747),
 .UNSPECIFIED.);
#467=B_SPLINE_CURVE_WITH_KNOTS('',3,(#25013,#25014,#25015,#25016),
 .UNSPECIFIED.,.F.,.F.,(4,4),(0.0319696744346003,0.0766821311551615),
 .UNSPECIFIED.);
#468=B_SPLINE_CURVE_WITH_KNOTS('',3,(#25017,#25018,#25019,#25020),
 .UNSPECIFIED.,.F.,.F.,(4,4),(0.0319696744346077,0.0766821311551524),
 .UNSPECIFIED.);
#469=B_SPLINE_CURVE_WITH_KNOTS('',3,(#25055,#25056,#25057,#25058),
 .UNSPECIFIED.,.F.,.F.,(4,4),(0.0319696744346155,0.0766821311551595),
 .UNSPECIFIED.);
#470=B_SPLINE_CURVE_WITH_KNOTS('',3,(#25059,#25060,#25061,#25062),
 .UNSPECIFIED.,.F.,.F.,(4,4),(0.0319696744346145,0.0766821311551639),
 .UNSPECIFIED.);
#471=B_SPLINE_CURVE_WITH_KNOTS('',3,(#25097,#25098,#25099,#25100),
 .UNSPECIFIED.,.F.,.F.,(4,4),(0.0319696744346048,0.0766821311551673),
 .UNSPECIFIED.);
#472=B_SPLINE_CURVE_WITH_KNOTS('',3,(#25101,#25102,#25103,#25104),
 .UNSPECIFIED.,.F.,.F.,(4,4),(0.0319696744346148,0.0766821311551611),
 .UNSPECIFIED.);
#473=B_SPLINE_CURVE_WITH_KNOTS('',3,(#25147,#25148,#25149,#25150),
 .UNSPECIFIED.,.F.,.F.,(4,4),(0.0319696744346167,0.0766821311551506),
 .UNSPECIFIED.);
#474=B_SPLINE_CURVE_WITH_KNOTS('',3,(#25151,#25152,#25153,#25154),
 .UNSPECIFIED.,.F.,.F.,(4,4),(0.0773553082819305,0.0893225623759919),
 .UNSPECIFIED.);
#475=B_SPLINE_CURVE_WITH_KNOTS('',3,(#25189,#25190,#25191,#25192),
 .UNSPECIFIED.,.F.,.F.,(4,4),(0.0319696744346161,0.0766821311551558),
 .UNSPECIFIED.);
#476=B_SPLINE_CURVE_WITH_KNOTS('',3,(#25193,#25194,#25195,#25196),
 .UNSPECIFIED.,.F.,.F.,(4,4),(0.031969674434606,0.0766821311551616),
 .UNSPECIFIED.);
#477=B_SPLINE_CURVE_WITH_KNOTS('',3,(#25231,#25232,#25233,#25234),
 .UNSPECIFIED.,.F.,.F.,(4,4),(0.031969674434617,0.0766821311551659),
 .UNSPECIFIED.);
#478=B_SPLINE_CURVE_WITH_KNOTS('',3,(#25235,#25236,#25237,#25238),
 .UNSPECIFIED.,.F.,.F.,(4,4),(0.0319696744346159,0.0766821311551567),
 .UNSPECIFIED.);
#479=B_SPLINE_CURVE_WITH_KNOTS('',3,(#25273,#25274,#25275,#25276),
 .UNSPECIFIED.,.F.,.F.,(4,4),(0.0319696744346169,0.0766821311551513),
 .UNSPECIFIED.);
#480=B_SPLINE_CURVE_WITH_KNOTS('',3,(#25277,#25278,#25279,#25280),
 .UNSPECIFIED.,.F.,.F.,(4,4),(0.0319696744346152,0.0766821311551648),
 .UNSPECIFIED.);
#481=B_SPLINE_CURVE_WITH_KNOTS('',3,(#25315,#25316,#25317,#25318),
 .UNSPECIFIED.,.F.,.F.,(4,4),(0.0319696744346174,0.0766821311551486),
 .UNSPECIFIED.);
#482=B_SPLINE_CURVE_WITH_KNOTS('',3,(#25319,#25320,#25321,#25322),
 .UNSPECIFIED.,.F.,.F.,(4,4),(0.0319696744346054,0.0766821311551601),
 .UNSPECIFIED.);
#483=B_SPLINE_CURVE_WITH_KNOTS('',3,(#25357,#25358,#25359,#25360),
 .UNSPECIFIED.,.F.,.F.,(4,4),(0.165217092335987,0.177184346430039),
 .UNSPECIFIED.);
#484=B_SPLINE_CURVE_WITH_KNOTS('',3,(#25361,#25362,#25363,#25364),
 .UNSPECIFIED.,.F.,.F.,(4,4),(0.0319696744346053,0.0766821311551563),
 .UNSPECIFIED.);
#485=B_SPLINE_CURVE_WITH_KNOTS('',3,(#25377,#25378,#25379,#25380),
 .UNSPECIFIED.,.F.,.F.,(4,4),(0.,0.0964441447213629),.UNSPECIFIED.);
#486=B_SPLINE_CURVE_WITH_KNOTS('',3,(#25382,#25383,#25384,#25385),
 .UNSPECIFIED.,.F.,.F.,(4,4),(-0.0893225623759869,-0.0773554379396867),
 .UNSPECIFIED.);
#487=B_SPLINE_CURVE_WITH_KNOTS('',3,(#25445,#25446,#25447,#25448),
 .UNSPECIFIED.,.F.,.F.,(4,4),(0.,0.0446132763744278),.UNSPECIFIED.);
#488=B_SPLINE_CURVE_WITH_KNOTS('',3,(#25449,#25450,#25451,#25452),
 .UNSPECIFIED.,.F.,.F.,(4,4),(0.0319696744346159,0.0766821311551664),
 .UNSPECIFIED.);
#489=B_SPLINE_CURVE_WITH_KNOTS('',3,(#25472,#25473,#25474,#25475),
 .UNSPECIFIED.,.F.,.F.,(4,4),(0.0319696744346157,0.0766821311551561),
 .UNSPECIFIED.);
#490=B_SPLINE_CURVE_WITH_KNOTS('',3,(#25493,#25494,#25495,#25496),
 .UNSPECIFIED.,.F.,.F.,(4,4),(0.0319696744346008,0.076682131155157),
 .UNSPECIFIED.);
#491=B_SPLINE_CURVE_WITH_KNOTS('',3,(#25531,#25532,#25533,#25534),
 .UNSPECIFIED.,.F.,.F.,(4,4),(0.0319696744346162,0.0766821311551517),
 .UNSPECIFIED.);
#492=B_SPLINE_CURVE_WITH_KNOTS('',3,(#25535,#25536,#25537,#25538),
 .UNSPECIFIED.,.F.,.F.,(4,4),(0.031969674434614,0.0766821311551579),
 .UNSPECIFIED.);
#493=B_SPLINE_CURVE_WITH_KNOTS('',3,(#25573,#25574,#25575,#25576),
 .UNSPECIFIED.,.F.,.F.,(4,4),(0.0319696744346152,0.0766821311551576),
 .UNSPECIFIED.);
#494=B_SPLINE_CURVE_WITH_KNOTS('',3,(#25577,#25578,#25579,#25580),
 .UNSPECIFIED.,.F.,.F.,(4,4),(0.0319696744346146,0.076682131155164),
 .UNSPECIFIED.);
#495=B_SPLINE_CURVE_WITH_KNOTS('',3,(#25603,#25604,#25605,#25606),
 .UNSPECIFIED.,.F.,.F.,(4,4),(0.165217092335987,0.177184346430036),
 .UNSPECIFIED.);
#496=B_SPLINE_CURVE_WITH_KNOTS('',3,(#25630,#25631,#25632,#25633),
 .UNSPECIFIED.,.F.,.F.,(4,4),(0.0319696744346059,0.0766821311551569),
 .UNSPECIFIED.);
#497=B_SPLINE_CURVE_WITH_KNOTS('',3,(#25634,#25635,#25636,#25637),
 .UNSPECIFIED.,.F.,.F.,(4,4),(0.0773553082819314,0.0893225623759902),
 .UNSPECIFIED.);
#498=B_SPLINE_CURVE_WITH_KNOTS('',3,(#25672,#25673,#25674,#25675),
 .UNSPECIFIED.,.F.,.F.,(4,4),(0.0319696744345999,0.0766821311551614),
 .UNSPECIFIED.);
#499=B_SPLINE_CURVE_WITH_KNOTS('',3,(#25676,#25677,#25678,#25679),
 .UNSPECIFIED.,.F.,.F.,(4,4),(0.0319696744346005,0.0766821311551545),
 .UNSPECIFIED.);
#500=B_SPLINE_CURVE_WITH_KNOTS('',3,(#25714,#25715,#25716,#25717),
 .UNSPECIFIED.,.F.,.F.,(4,4),(0.0319696744346044,0.0766821311551586),
 .UNSPECIFIED.);
#501=B_SPLINE_CURVE_WITH_KNOTS('',3,(#25718,#25719,#25720,#25721),
 .UNSPECIFIED.,.F.,.F.,(4,4),(0.0319696744346146,0.0766821311551602),
 .UNSPECIFIED.);
#502=B_SPLINE_CURVE_WITH_KNOTS('',3,(#25756,#25757,#25758,#25759),
 .UNSPECIFIED.,.F.,.F.,(4,4),(0.0319696744345999,0.0766821311551589),
 .UNSPECIFIED.);
#503=B_SPLINE_CURVE_WITH_KNOTS('',3,(#25760,#25761,#25762,#25763),
 .UNSPECIFIED.,.F.,.F.,(4,4),(0.0319696744346151,0.0766821311551586),
 .UNSPECIFIED.);
#504=B_SPLINE_CURVE_WITH_KNOTS('',3,(#25798,#25799,#25800,#25801),
 .UNSPECIFIED.,.F.,.F.,(4,4),(0.165217092335985,0.177184346430047),
 .UNSPECIFIED.);
#505=B_SPLINE_CURVE_WITH_KNOTS('',3,(#25802,#25803,#25804,#25805),
 .UNSPECIFIED.,.F.,.F.,(4,4),(0.,0.0446132763744527),.UNSPECIFIED.);
#506=B_SPLINE_CURVE_WITH_KNOTS('',3,(#25818,#25819,#25820,#25821),
 .UNSPECIFIED.,.F.,.F.,(4,4),(0.,0.0964441447213381),.UNSPECIFIED.);
#507=B_SPLINE_CURVE_WITH_KNOTS('',3,(#25823,#25824,#25825,#25826),
 .UNSPECIFIED.,.F.,.F.,(4,4),(-0.0893225623759864,-0.0773554379396737),
 .UNSPECIFIED.);
#508=B_SPLINE_CURVE_WITH_KNOTS('',3,(#25884,#25885,#25886,#25887),
 .UNSPECIFIED.,.F.,.F.,(4,4),(0.0319696744346151,0.0766821311551646),
 .UNSPECIFIED.);
#509=B_SPLINE_CURVE_WITH_KNOTS('',3,(#25888,#25889,#25890,#25891),
 .UNSPECIFIED.,.F.,.F.,(4,4),(0.0319696744346152,0.0766821311551612),
 .UNSPECIFIED.);
#510=B_SPLINE_CURVE_WITH_KNOTS('',3,(#25926,#25927,#25928,#25929),
 .UNSPECIFIED.,.F.,.F.,(4,4),(0.031969674434616,0.0766821311551564),
 .UNSPECIFIED.);
#511=B_SPLINE_CURVE_WITH_KNOTS('',3,(#25930,#25931,#25932,#25933),
 .UNSPECIFIED.,.F.,.F.,(4,4),(0.0319696744346053,0.0766821311551682),
 .UNSPECIFIED.);
#512=B_SPLINE_CURVE_WITH_KNOTS('',3,(#25968,#25969,#25970,#25971),
 .UNSPECIFIED.,.F.,.F.,(4,4),(0.0319696744346154,0.0766821311551632),
 .UNSPECIFIED.);
#513=B_SPLINE_CURVE_WITH_KNOTS('',3,(#25972,#25973,#25974,#25975),
 .UNSPECIFIED.,.F.,.F.,(4,4),(0.0319696744346182,0.0766821311551516),
 .UNSPECIFIED.);
#514=B_SPLINE_CURVE_WITH_KNOTS('',3,(#26010,#26011,#26012,#26013),
 .UNSPECIFIED.,.F.,.F.,(4,4),(0.0319696744346054,0.076682131155166),
 .UNSPECIFIED.);
#515=B_SPLINE_CURVE_WITH_KNOTS('',3,(#26014,#26015,#26016,#26017),
 .UNSPECIFIED.,.F.,.F.,(4,4),(0.0319696744346067,0.0766821311551598),
 .UNSPECIFIED.);
#516=B_SPLINE_CURVE_WITH_KNOTS('',3,(#26052,#26053,#26054,#26055),
 .UNSPECIFIED.,.F.,.F.,(4,4),(0.0319696744346162,0.0766821311551578),
 .UNSPECIFIED.);
#517=B_SPLINE_CURVE_WITH_KNOTS('',3,(#26056,#26057,#26058,#26059),
 .UNSPECIFIED.,.F.,.F.,(4,4),(0.0319696744346034,0.0766821311551686),
 .UNSPECIFIED.);
#518=B_SPLINE_CURVE_WITH_KNOTS('',3,(#26082,#26083,#26084,#26085),
 .UNSPECIFIED.,.F.,.F.,(4,4),(0.165217092335987,0.17718434643005),
 .UNSPECIFIED.);
#519=B_SPLINE_CURVE_WITH_KNOTS('',3,(#26109,#26110,#26111,#26112),
 .UNSPECIFIED.,.F.,.F.,(4,4),(0.0319696744346091,0.0766821311551474),
 .UNSPECIFIED.);
#520=B_SPLINE_CURVE_WITH_KNOTS('',3,(#26113,#26114,#26115,#26116),
 .UNSPECIFIED.,.F.,.F.,(4,4),(0.077355308281932,0.0893225623759954),
 .UNSPECIFIED.);
#521=B_SPLINE_CURVE_WITH_KNOTS('',3,(#26151,#26152,#26153,#26154),
 .UNSPECIFIED.,.F.,.F.,(4,4),(0.0319696744346146,0.0766821311551647),
 .UNSPECIFIED.);
#522=B_SPLINE_CURVE_WITH_KNOTS('',3,(#26155,#26156,#26157,#26158),
 .UNSPECIFIED.,.F.,.F.,(4,4),(0.0319696744346137,0.0766821311551644),
 .UNSPECIFIED.);
#523=B_SPLINE_CURVE_WITH_KNOTS('',3,(#26193,#26194,#26195,#26196),
 .UNSPECIFIED.,.F.,.F.,(4,4),(0.0319696744346069,0.0766821311551582),
 .UNSPECIFIED.);
#524=B_SPLINE_CURVE_WITH_KNOTS('',3,(#26197,#26198,#26199,#26200),
 .UNSPECIFIED.,.F.,.F.,(4,4),(0.0319696744346155,0.0766821311551643),
 .UNSPECIFIED.);
#525=B_SPLINE_CURVE_WITH_KNOTS('',3,(#26235,#26236,#26237,#26238),
 .UNSPECIFIED.,.F.,.F.,(4,4),(0.165217092335985,0.177184346430037),
 .UNSPECIFIED.);
#526=B_SPLINE_CURVE_WITH_KNOTS('',3,(#26239,#26240,#26241,#26242),
 .UNSPECIFIED.,.F.,.F.,(4,4),(0.031969674434605,0.0766821311551589),
 .UNSPECIFIED.);
#527=B_SPLINE_CURVE_WITH_KNOTS('',3,(#26255,#26256,#26257,#26258),
 .UNSPECIFIED.,.F.,.F.,(4,4),(0.,0.0964441447218811),.UNSPECIFIED.);
#528=B_SPLINE_CURVE_WITH_KNOTS('',3,(#26260,#26261,#26262,#26263),
 .UNSPECIFIED.,.F.,.F.,(4,4),(-0.0893225623759877,-0.0773554379396747),
 .UNSPECIFIED.);
#529=B_SPLINE_CURVE_WITH_KNOTS('',3,(#26323,#26324,#26325,#26326),
 .UNSPECIFIED.,.F.,.F.,(4,4),(0.,0.0446132763744454),.UNSPECIFIED.);
#530=B_SPLINE_CURVE_WITH_KNOTS('',3,(#26327,#26328,#26329,#26330),
 .UNSPECIFIED.,.F.,.F.,(4,4),(0.0319696744346051,0.0766821311551664),
 .UNSPECIFIED.);
#531=B_SPLINE_CURVE_WITH_KNOTS('',3,(#26350,#26351,#26352,#26353),
 .UNSPECIFIED.,.F.,.F.,(4,4),(0.0319696744346155,0.0766821311551594),
 .UNSPECIFIED.);
#532=B_SPLINE_CURVE_WITH_KNOTS('',3,(#26371,#26372,#26373,#26374),
 .UNSPECIFIED.,.F.,.F.,(4,4),(0.0319696744346062,0.0766821311551557),
 .UNSPECIFIED.);
#533=B_SPLINE_CURVE_WITH_KNOTS('',3,(#26409,#26410,#26411,#26412),
 .UNSPECIFIED.,.F.,.F.,(4,4),(0.0319696744346158,0.07668213115516),
 .UNSPECIFIED.);
#534=B_SPLINE_CURVE_WITH_KNOTS('',3,(#26413,#26414,#26415,#26416),
 .UNSPECIFIED.,.F.,.F.,(4,4),(0.0319696744346155,0.0766821311551679),
 .UNSPECIFIED.);
#535=B_SPLINE_CURVE_WITH_KNOTS('',3,(#26451,#26452,#26453,#26454),
 .UNSPECIFIED.,.F.,.F.,(4,4),(0.0319696744346141,0.0766821311551622),
 .UNSPECIFIED.);
#536=B_SPLINE_CURVE_WITH_KNOTS('',3,(#26455,#26456,#26457,#26458),
 .UNSPECIFIED.,.F.,.F.,(4,4),(0.0319696744346023,0.0766821311551525),
 .UNSPECIFIED.);
#537=B_SPLINE_CURVE_WITH_KNOTS('',3,(#26493,#26494,#26495,#26496),
 .UNSPECIFIED.,.F.,.F.,(4,4),(0.0319696744346052,0.0766821311551627),
 .UNSPECIFIED.);
#538=B_SPLINE_CURVE_WITH_KNOTS('',3,(#26497,#26498,#26499,#26500),
 .UNSPECIFIED.,.F.,.F.,(4,4),(0.031969674434614,0.076682131155166),
 .UNSPECIFIED.);
#539=B_SPLINE_CURVE_WITH_KNOTS('',3,(#26535,#26536,#26537,#26538),
 .UNSPECIFIED.,.F.,.F.,(4,4),(0.0319696744345985,0.0766821311551622),
 .UNSPECIFIED.);
#540=B_SPLINE_CURVE_WITH_KNOTS('',3,(#26539,#26540,#26541,#26542),
 .UNSPECIFIED.,.F.,.F.,(4,4),(0.031969674434617,0.0766821311551562),
 .UNSPECIFIED.);
#541=B_SPLINE_CURVE_WITH_KNOTS('',3,(#26565,#26566,#26567,#26568),
 .UNSPECIFIED.,.F.,.F.,(4,4),(0.165217092335983,0.177184346430045),
 .UNSPECIFIED.);
#542=B_SPLINE_CURVE_WITH_KNOTS('',3,(#26592,#26593,#26594,#26595),
 .UNSPECIFIED.,.F.,.F.,(4,4),(0.0319696744346161,0.0766821311551627),
 .UNSPECIFIED.);
#543=B_SPLINE_CURVE_WITH_KNOTS('',3,(#26596,#26597,#26598,#26599),
 .UNSPECIFIED.,.F.,.F.,(4,4),(0.0773553082819429,0.089322562375992),
 .UNSPECIFIED.);
#544=B_SPLINE_CURVE_WITH_KNOTS('',3,(#26634,#26635,#26636,#26637),
 .UNSPECIFIED.,.F.,.F.,(4,4),(0.0319696744346067,0.0766821311551616),
 .UNSPECIFIED.);
#545=B_SPLINE_CURVE_WITH_KNOTS('',3,(#26638,#26639,#26640,#26641),
 .UNSPECIFIED.,.F.,.F.,(4,4),(0.0319696744346059,0.0766821311551612),
 .UNSPECIFIED.);
#546=B_SPLINE_CURVE_WITH_KNOTS('',3,(#26676,#26677,#26678,#26679),
 .UNSPECIFIED.,.F.,.F.,(4,4),(0.165217092335982,0.177184346430035),
 .UNSPECIFIED.);
#547=B_SPLINE_CURVE_WITH_KNOTS('',3,(#26680,#26681,#26682,#26683),
 .UNSPECIFIED.,.F.,.F.,(4,4),(0.,0.0446132763744144),.UNSPECIFIED.);
#548=B_SPLINE_CURVE_WITH_KNOTS('',3,(#26696,#26697,#26698,#26699),
 .UNSPECIFIED.,.F.,.F.,(4,4),(0.,0.0964441447215326),.UNSPECIFIED.);
#549=B_SPLINE_CURVE_WITH_KNOTS('',3,(#26701,#26702,#26703,#26704),
 .UNSPECIFIED.,.F.,.F.,(4,4),(-0.0893225623759896,-0.077355437939685),
 .UNSPECIFIED.);
#550=B_SPLINE_CURVE_WITH_KNOTS('',3,(#26762,#26763,#26764,#26765),
 .UNSPECIFIED.,.F.,.F.,(4,4),(0.0319696744346159,0.0766821311551599),
 .UNSPECIFIED.);
#551=B_SPLINE_CURVE_WITH_KNOTS('',3,(#26766,#26767,#26768,#26769),
 .UNSPECIFIED.,.F.,.F.,(4,4),(0.0319696744346145,0.0766821311551639),
 .UNSPECIFIED.);
#552=B_SPLINE_CURVE_WITH_KNOTS('',3,(#26804,#26805,#26806,#26807),
 .UNSPECIFIED.,.F.,.F.,(4,4),(0.0319696744346048,0.0766821311551603),
 .UNSPECIFIED.);
#553=B_SPLINE_CURVE_WITH_KNOTS('',3,(#26808,#26809,#26810,#26811),
 .UNSPECIFIED.,.F.,.F.,(4,4),(0.0319696744346048,0.0766821311551578),
 .UNSPECIFIED.);
#554=B_SPLINE_CURVE_WITH_KNOTS('',3,(#26846,#26847,#26848,#26849),
 .UNSPECIFIED.,.F.,.F.,(4,4),(0.0319696744346148,0.0766821311551675),
 .UNSPECIFIED.);
#555=B_SPLINE_CURVE_WITH_KNOTS('',3,(#26850,#26851,#26852,#26853),
 .UNSPECIFIED.,.F.,.F.,(4,4),(0.0319696744346143,0.0766821311551628),
 .UNSPECIFIED.);
#556=B_SPLINE_CURVE_WITH_KNOTS('',3,(#26888,#26889,#26890,#26891),
 .UNSPECIFIED.,.F.,.F.,(4,4),(0.031969674434616,0.07668213115516),
 .UNSPECIFIED.);
#557=B_SPLINE_CURVE_WITH_KNOTS('',3,(#26892,#26893,#26894,#26895),
 .UNSPECIFIED.,.F.,.F.,(4,4),(0.0319696744346167,0.0766821311551533),
 .UNSPECIFIED.);
#558=B_SPLINE_CURVE_WITH_KNOTS('',3,(#26930,#26931,#26932,#26933),
 .UNSPECIFIED.,.F.,.F.,(4,4),(0.031969674434616,0.0766821311551576),
 .UNSPECIFIED.);
#559=B_SPLINE_CURVE_WITH_KNOTS('',3,(#26934,#26935,#26936,#26937),
 .UNSPECIFIED.,.F.,.F.,(4,4),(0.0319696744346139,0.0766821311551655),
 .UNSPECIFIED.);
#560=B_SPLINE_CURVE_WITH_KNOTS('',3,(#26972,#26973,#26974,#26975),
 .UNSPECIFIED.,.F.,.F.,(4,4),(0.0319696744346157,0.0766821311551638),
 .UNSPECIFIED.);
#561=B_SPLINE_CURVE_WITH_KNOTS('',3,(#26976,#26977,#26978,#26979),
 .UNSPECIFIED.,.F.,.F.,(4,4),(0.0319696744346155,0.0766821311551616),
 .UNSPECIFIED.);
#562=B_SPLINE_CURVE_WITH_KNOTS('',3,(#27014,#27015,#27016,#27017),
 .UNSPECIFIED.,.F.,.F.,(4,4),(0.0319696744346065,0.0766821311551571),
 .UNSPECIFIED.);
#563=B_SPLINE_CURVE_WITH_KNOTS('',3,(#27018,#27019,#27020,#27021),
 .UNSPECIFIED.,.F.,.F.,(4,4),(0.0319696744346042,0.0766821311551645),
 .UNSPECIFIED.);
#564=B_SPLINE_CURVE_WITH_KNOTS('',3,(#27044,#27045,#27046,#27047),
 .UNSPECIFIED.,.F.,.F.,(4,4),(0.165217092335988,0.177184346430048),
 .UNSPECIFIED.);
#565=B_SPLINE_CURVE_WITH_KNOTS('',3,(#27071,#27072,#27073,#27074),
 .UNSPECIFIED.,.F.,.F.,(4,4),(0.0319696744346034,0.0766821311551701),
 .UNSPECIFIED.);
#566=B_SPLINE_CURVE_WITH_KNOTS('',3,(#27075,#27076,#27077,#27078),
 .UNSPECIFIED.,.F.,.F.,(4,4),(0.0773553082819422,0.0893225623759928),
 .UNSPECIFIED.);
#567=B_SPLINE_CURVE_WITH_KNOTS('',3,(#27113,#27114,#27115,#27116),
 .UNSPECIFIED.,.F.,.F.,(4,4),(0.165217092335984,0.177184346430047),
 .UNSPECIFIED.);
#568=B_SPLINE_CURVE_WITH_KNOTS('',3,(#27117,#27118,#27119,#27120),
 .UNSPECIFIED.,.F.,.F.,(4,4),(0.0319696744346047,0.0766821311551648),
 .UNSPECIFIED.);
#569=B_SPLINE_CURVE_WITH_KNOTS('',3,(#27133,#27134,#27135,#27136),
 .UNSPECIFIED.,.F.,.F.,(4,4),(0.,0.0964441447216793),.UNSPECIFIED.);
#570=B_SPLINE_CURVE_WITH_KNOTS('',3,(#27138,#27139,#27140,#27141),
 .UNSPECIFIED.,.F.,.F.,(4,4),(-0.0893225623759868,-0.077355437939685),
 .UNSPECIFIED.);
#571=B_SPLINE_CURVE_WITH_KNOTS('',3,(#27201,#27202,#27203,#27204),
 .UNSPECIFIED.,.F.,.F.,(4,4),(0.0319696744346011,0.0766821311551579),
 .UNSPECIFIED.);
#572=B_SPLINE_CURVE_WITH_KNOTS('',3,(#27205,#27206,#27207,#27208),
 .UNSPECIFIED.,.F.,.F.,(4,4),(0.031969674434615,0.0766821311551662),
 .UNSPECIFIED.);
#573=B_SPLINE_CURVE_WITH_KNOTS('',3,(#27243,#27244,#27245,#27246),
 .UNSPECIFIED.,.F.,.F.,(4,4),(0.0319696744346163,0.0766821311551522),
 .UNSPECIFIED.);
#574=B_SPLINE_CURVE_WITH_KNOTS('',3,(#27247,#27248,#27249,#27250),
 .UNSPECIFIED.,.F.,.F.,(4,4),(0.0319696744346142,0.0766821311551595),
 .UNSPECIFIED.);
#575=B_SPLINE_CURVE_WITH_KNOTS('',3,(#27285,#27286,#27287,#27288),
 .UNSPECIFIED.,.F.,.F.,(4,4),(0.0319696744346053,0.0766821311551585),
 .UNSPECIFIED.);
#576=B_SPLINE_CURVE_WITH_KNOTS('',3,(#27289,#27290,#27291,#27292),
 .UNSPECIFIED.,.F.,.F.,(4,4),(0.0319696744346046,0.0766821311551665),
 .UNSPECIFIED.);
#577=B_SPLINE_CURVE_WITH_KNOTS('',3,(#27327,#27328,#27329,#27330),
 .UNSPECIFIED.,.F.,.F.,(4,4),(0.0319696744346158,0.0766821311551619),
 .UNSPECIFIED.);
#578=B_SPLINE_CURVE_WITH_KNOTS('',3,(#27331,#27332,#27333,#27334),
 .UNSPECIFIED.,.F.,.F.,(4,4),(0.0319696744346162,0.0766821311551531),
 .UNSPECIFIED.);
#579=B_SPLINE_CURVE_WITH_KNOTS('',3,(#27369,#27370,#27371,#27372),
 .UNSPECIFIED.,.F.,.F.,(4,4),(0.0319696744346129,0.0766821311551683),
 .UNSPECIFIED.);
#580=B_SPLINE_CURVE_WITH_KNOTS('',3,(#27373,#27374,#27375,#27376),
 .UNSPECIFIED.,.F.,.F.,(4,4),(0.0319696744346159,0.0766821311551596),
 .UNSPECIFIED.);
#581=B_SPLINE_CURVE_WITH_KNOTS('',3,(#27411,#27412,#27413,#27414),
 .UNSPECIFIED.,.F.,.F.,(4,4),(0.0319696744346056,0.076682131155164),
 .UNSPECIFIED.);
#582=B_SPLINE_CURVE_WITH_KNOTS('',3,(#27415,#27416,#27417,#27418),
 .UNSPECIFIED.,.F.,.F.,(4,4),(0.031969674434616,0.0766821311551558),
 .UNSPECIFIED.);
#583=B_SPLINE_CURVE_WITH_KNOTS('',3,(#27453,#27454,#27455,#27456),
 .UNSPECIFIED.,.F.,.F.,(4,4),(0.0319696744346056,0.0766821311551581),
 .UNSPECIFIED.);
#584=B_SPLINE_CURVE_WITH_KNOTS('',3,(#27457,#27458,#27459,#27460),
 .UNSPECIFIED.,.F.,.F.,(4,4),(0.0319696744346045,0.0766821311551705),
 .UNSPECIFIED.);
#585=B_SPLINE_CURVE_WITH_KNOTS('',3,(#27495,#27496,#27497,#27498),
 .UNSPECIFIED.,.F.,.F.,(4,4),(0.0319696744346149,0.0766821311551601),
 .UNSPECIFIED.);
#586=B_SPLINE_CURVE_WITH_KNOTS('',3,(#27499,#27500,#27501,#27502),
 .UNSPECIFIED.,.F.,.F.,(4,4),(0.0319696744346128,0.0766821311551717),
 .UNSPECIFIED.);
#587=B_SPLINE_CURVE_WITH_KNOTS('',3,(#27525,#27526,#27527,#27528),
 .UNSPECIFIED.,.F.,.F.,(4,4),(0.165217092335982,0.177184346430046),
 .UNSPECIFIED.);
#588=B_SPLINE_CURVE_WITH_KNOTS('',3,(#27552,#27553,#27554,#27555),
 .UNSPECIFIED.,.F.,.F.,(4,4),(0.165217092335986,0.177184346430048),
 .UNSPECIFIED.);
#589=B_SPLINE_CURVE_WITH_KNOTS('',3,(#27556,#27557,#27558,#27559),
 .UNSPECIFIED.,.F.,.F.,(4,4),(0.077355308281931,0.0893225623759923),
 .UNSPECIFIED.);
#590=B_SPLINE_CURVE_WITH_KNOTS('',3,(#27572,#27573,#27574,#27575),
 .UNSPECIFIED.,.F.,.F.,(4,4),(0.,0.096444144720994),.UNSPECIFIED.);
#591=B_SPLINE_CURVE_WITH_KNOTS('',3,(#27577,#27578,#27579,#27580),
 .UNSPECIFIED.,.F.,.F.,(4,4),(-0.0893225623759868,-0.0773554379396859),
 .UNSPECIFIED.);
#592=B_SPLINE_CURVE_WITH_KNOTS('',3,(#27635,#27636,#27637,#27638),
 .UNSPECIFIED.,.F.,.F.,(4,4),(0.0319696744346056,0.0766821311551627),
 .UNSPECIFIED.);
#593=B_SPLINE_CURVE_WITH_KNOTS('',3,(#27673,#27674,#27675,#27676),
 .UNSPECIFIED.,.F.,.F.,(4,4),(0.0319696744346165,0.0766821311551601),
 .UNSPECIFIED.);
#594=B_SPLINE_CURVE_WITH_KNOTS('',3,(#27677,#27678,#27679,#27680),
 .UNSPECIFIED.,.F.,.F.,(4,4),(0.0319696744346167,0.0766821311551504),
 .UNSPECIFIED.);
#595=B_SPLINE_CURVE_WITH_KNOTS('',3,(#27715,#27716,#27717,#27718),
 .UNSPECIFIED.,.F.,.F.,(4,4),(0.031969674434606,0.0766821311551567),
 .UNSPECIFIED.);
#596=B_SPLINE_CURVE_WITH_KNOTS('',3,(#27719,#27720,#27721,#27722),
 .UNSPECIFIED.,.F.,.F.,(4,4),(0.0319696744346156,0.0766821311551527),
 .UNSPECIFIED.);
#597=B_SPLINE_CURVE_WITH_KNOTS('',3,(#27757,#27758,#27759,#27760),
 .UNSPECIFIED.,.F.,.F.,(4,4),(0.0319696744346135,0.0766821311551671),
 .UNSPECIFIED.);
#598=B_SPLINE_CURVE_WITH_KNOTS('',3,(#27761,#27762,#27763,#27764),
 .UNSPECIFIED.,.F.,.F.,(4,4),(0.0319696744346146,0.076682131155166),
 .UNSPECIFIED.);
#599=B_SPLINE_CURVE_WITH_KNOTS('',3,(#27799,#27800,#27801,#27802),
 .UNSPECIFIED.,.F.,.F.,(4,4),(0.0319696744346137,0.0766821311551702),
 .UNSPECIFIED.);
#600=B_SPLINE_CURVE_WITH_KNOTS('',3,(#27803,#27804,#27805,#27806),
 .UNSPECIFIED.,.F.,.F.,(4,4),(0.0319696744346153,0.0766821311551645),
 .UNSPECIFIED.);
#601=B_SPLINE_CURVE_WITH_KNOTS('',3,(#27841,#27842,#27843,#27844),
 .UNSPECIFIED.,.F.,.F.,(4,4),(0.0319696744346044,0.0766821311551661),
 .UNSPECIFIED.);
#602=B_SPLINE_CURVE_WITH_KNOTS('',3,(#27845,#27846,#27847,#27848),
 .UNSPECIFIED.,.F.,.F.,(4,4),(0.031969674434616,0.0766821311551596),
 .UNSPECIFIED.);
#603=B_SPLINE_CURVE_WITH_KNOTS('',3,(#27883,#27884,#27885,#27886),
 .UNSPECIFIED.,.F.,.F.,(4,4),(0.0319696744346171,0.0766821311551567),
 .UNSPECIFIED.);
#604=B_SPLINE_CURVE_WITH_KNOTS('',3,(#27887,#27888,#27889,#27890),
 .UNSPECIFIED.,.F.,.F.,(4,4),(0.0319696744346159,0.0766821311551545),
 .UNSPECIFIED.);
#605=B_SPLINE_CURVE_WITH_KNOTS('',3,(#27925,#27926,#27927,#27928),
 .UNSPECIFIED.,.F.,.F.,(4,4),(0.0319696744346147,0.0766821311551627),
 .UNSPECIFIED.);
#606=B_SPLINE_CURVE_WITH_KNOTS('',3,(#27929,#27930,#27931,#27932),
 .UNSPECIFIED.,.F.,.F.,(4,4),(0.031969674434614,0.0766821311551628),
 .UNSPECIFIED.);
#607=B_SPLINE_CURVE_WITH_KNOTS('',3,(#27967,#27968,#27969,#27970),
 .UNSPECIFIED.,.F.,.F.,(4,4),(0.0319696744346007,0.0766821311551619),
 .UNSPECIFIED.);
#608=B_SPLINE_CURVE_WITH_KNOTS('',3,(#27971,#27972,#27973,#27974),
 .UNSPECIFIED.,.F.,.F.,(4,4),(0.0319696744346149,0.0766821311551584),
 .UNSPECIFIED.);
#609=B_SPLINE_CURVE_WITH_KNOTS('',3,(#28090,#28091,#28092,#28093),
 .UNSPECIFIED.,.F.,.F.,(4,4),(0.,0.0964441447212768),.UNSPECIFIED.);
#610=B_SPLINE_CURVE_WITH_KNOTS('',3,(#28098,#28099,#28100,#28101),
 .UNSPECIFIED.,.F.,.F.,(4,4),(0.,0.0964441447214986),.UNSPECIFIED.);
#611=B_SPLINE_CURVE_WITH_KNOTS('',3,(#28102,#28103,#28104,#28105),
 .UNSPECIFIED.,.F.,.F.,(4,4),(0.336279561120233,0.34824668540691),
 .UNSPECIFIED.);
#612=B_SPLINE_CURVE_WITH_KNOTS('',3,(#28117,#28118,#28119,#28120),
 .UNSPECIFIED.,.F.,.F.,(4,4),(-0.0893225623759864,-0.0773554379396748),
 .UNSPECIFIED.);
#613=B_SPLINE_CURVE_WITH_KNOTS('',3,(#28129,#28130,#28131,#28132),
 .UNSPECIFIED.,.F.,.F.,(4,4),(0.,0.0964441447214225),.UNSPECIFIED.);
#614=B_SPLINE_CURVE_WITH_KNOTS('',3,(#28136,#28137,#28138,#28139),
 .UNSPECIFIED.,.F.,.F.,(4,4),(0.,0.096444144721337),.UNSPECIFIED.);
#615=B_SPLINE_CURVE_WITH_KNOTS('',3,(#28140,#28141,#28142,#28143),
 .UNSPECIFIED.,.F.,.F.,(4,4),(-0.0893225623759897,-0.0773554379396767),
 .UNSPECIFIED.);
#616=B_SPLINE_CURVE_WITH_KNOTS('',3,(#28150,#28151,#28152,#28153),
 .UNSPECIFIED.,.F.,.F.,(4,4),(-0.177184216772303,-0.165217092335987),
 .UNSPECIFIED.);
#617=B_SPLINE_CURVE_WITH_KNOTS('',3,(#28162,#28163,#28164,#28165),
 .UNSPECIFIED.,.F.,.F.,(4,4),(0.,0.0964441447210733),.UNSPECIFIED.);
#618=B_SPLINE_CURVE_WITH_KNOTS('',3,(#28170,#28171,#28172,#28173),
 .UNSPECIFIED.,.F.,.F.,(4,4),(0.,0.0964441447210223),.UNSPECIFIED.);
#619=B_SPLINE_CURVE_WITH_KNOTS('',3,(#28174,#28175,#28176,#28177),
 .UNSPECIFIED.,.F.,.F.,(4,4),(-0.177184216772304,-0.165217092335993),
 .UNSPECIFIED.);
#620=B_SPLINE_CURVE_WITH_KNOTS('',3,(#28189,#28190,#28191,#28192),
 .UNSPECIFIED.,.F.,.F.,(4,4),(-0.0893225623759886,-0.0773554379396872),
 .UNSPECIFIED.);
#621=B_SPLINE_CURVE_WITH_KNOTS('',3,(#28201,#28202,#28203,#28204),
 .UNSPECIFIED.,.F.,.F.,(4,4),(0.,0.0964441447215364),.UNSPECIFIED.);
#622=B_SPLINE_CURVE_WITH_KNOTS('',3,(#28208,#28209,#28210,#28211),
 .UNSPECIFIED.,.F.,.F.,(4,4),(0.,0.0964441447215273),.UNSPECIFIED.);
#623=B_SPLINE_CURVE_WITH_KNOTS('',3,(#28212,#28213,#28214,#28215),
 .UNSPECIFIED.,.F.,.F.,(4,4),(-0.0893225623759895,-0.077355437939685),
 .UNSPECIFIED.);
#624=B_SPLINE_CURVE_WITH_KNOTS('',3,(#28222,#28223,#28224,#28225),
 .UNSPECIFIED.,.F.,.F.,(4,4),(-0.177184216772292,-0.165217092335987),
 .UNSPECIFIED.);
#625=B_SPLINE_CURVE_WITH_KNOTS('',3,(#28234,#28235,#28236,#28237),
 .UNSPECIFIED.,.F.,.F.,(4,4),(0.,0.0964441447214411),.UNSPECIFIED.);
#626=B_SPLINE_CURVE_WITH_KNOTS('',3,(#28242,#28243,#28244,#28245),
 .UNSPECIFIED.,.F.,.F.,(4,4),(0.,0.0964441447215376),.UNSPECIFIED.);
#627=B_SPLINE_CURVE_WITH_KNOTS('',3,(#28246,#28247,#28248,#28249),
 .UNSPECIFIED.,.F.,.F.,(4,4),(-0.177184216772293,-0.165217092335991),
 .UNSPECIFIED.);
#628=B_SPLINE_CURVE_WITH_KNOTS('',3,(#28261,#28262,#28263,#28264),
 .UNSPECIFIED.,.F.,.F.,(4,4),(-0.0893225623759893,-0.0773554379396748),
 .UNSPECIFIED.);
#629=B_SPLINE_CURVE_WITH_KNOTS('',3,(#28270,#28271,#28272,#28273),
 .UNSPECIFIED.,.F.,.F.,(4,4),(0.,0.0964441447215519),.UNSPECIFIED.);
#630=B_SPLINE_CURVE_WITH_KNOTS('',3,(#28277,#28278,#28279,#28280),
 .UNSPECIFIED.,.F.,.F.,(4,4),(0.,0.0964441447216442),.UNSPECIFIED.);
#631=B_SPLINE_CURVE_WITH_KNOTS('',3,(#28607,#28608,#28609,#28610,#28611,
#28612,#28613,#28614,#28615,#28616,#28617,#28618,#28619,#28620,#28621,#28622,
#28623,#28624,#28625,#28626,#28627,#28628,#28629,#28630,#28631),
 .UNSPECIFIED.,.F.,.F.,(4,3,3,3,3,3,3,3,4),(-3.86638687953777,-3.47451718982531,
-2.97815759127883,-2.48179799273236,-1.98543839418589,-1.48907879563941,
-0.992719197092944,-0.496359598546473,0.),.UNSPECIFIED.);
#632=B_SPLINE_CURVE_WITH_KNOTS('',3,(#28634,#28635,#28636,#28637,#28638,
#28639,#28640,#28641,#28642,#28643,#28644,#28645,#28646,#28647,#28648,#28649,
#28650,#28651,#28652,#28653,#28654,#28655,#28656,#28657,#28658,#28659,#28660,
#28661,#28662,#28663,#28664,#28665,#28666,#28667,#28668,#28669,#28670),
 .UNSPECIFIED.,.F.,.F.,(4,3,3,3,3,3,3,3,3,3,3,3,4),(2.03387368709462,2.48179799273236,
2.97815759127883,3.4745171898253,3.97087678837177,4.46723638691825,4.96359598546472,
5.4599555840112,5.95631518255767,6.45267478110414,6.94903437965062,7.44539397819709,
7.59226476832617),.UNSPECIFIED.);
#633=B_SPLINE_CURVE_WITH_KNOTS('',3,(#28675,#28676,#28677,#28678,#28679,
#28680,#28681,#28682,#28683,#28684,#28685,#28686,#28687,#28688,#28689,#28690,
#28691,#28692,#28693,#28694,#28695,#28696,#28697,#28698,#28699,#28700,#28701,
#28702,#28703,#28704,#28705,#28706,#28707,#28708,#28709,#28710,#28711,#28712,
#28713,#28714,#28715,#28716,#28717),.UNSPECIFIED.,.F.,.F.,(4,3,3,3,3,3,
3,3,3,3,3,3,3,3,4),(-10.1495721867174,-9.92719197092945,-9.43083237238297,
-8.9344727738365,-8.43811317529003,-7.94175357674355,-7.44539397819708,
-6.94903437965061,-6.45267478110414,-5.95631518255767,-5.45995558401119,
-4.96359598546472,-4.46723638691825,-3.97087678837178,-3.86638687953777),
 .UNSPECIFIED.);
#634=B_SPLINE_CURVE_WITH_KNOTS('',3,(#28718,#28719,#28720,#28721,#28722,
#28723,#28724,#28725,#28726,#28727,#28728,#28729,#28730,#28731,#28732,#28733,
#28734,#28735,#28736,#28737,#28738,#28739,#28740,#28741,#28742,#28743,#28744,
#28745,#28746,#28747,#28748,#28749,#28750,#28751,#28752,#28753,#28754,#28755,
#28756,#28757),.UNSPECIFIED.,.F.,.F.,(4,3,3,3,3,3,3,3,3,3,3,3,3,4),(7.59226476832617,
7.94175357674356,8.43811317529003,8.93447277383651,9.43083237238297,9.92719197092945,
10.4235515694759,10.9199111680224,11.4162707665689,11.9126303651153,12.4089899636618,
12.9053495622083,13.4017091607548,13.8754500755058),.UNSPECIFIED.);
#635=B_SPLINE_CURVE_WITH_KNOTS('',3,(#28762,#28763,#28764,#28765,#28766,
#28767,#28768,#28769,#28770,#28771,#28772,#28773,#28774,#28775,#28776,#28777,
#28778,#28779,#28780,#28781,#28782,#28783,#28784,#28785,#28786,#28787,#28788,
#28789,#28790,#28791,#28792,#28793,#28794,#28795,#28796,#28797,#28798,#28799,
#28800,#28801,#28802,#28803,#28804),.UNSPECIFIED.,.F.,.F.,(4,3,3,3,3,3,
3,3,3,3,3,3,3,3,4),(-16.432757493897,-16.3798667520336,-15.8835071534871,
-15.3871475549406,-14.8907879563942,-14.3944283578477,-13.8980687593012,
-13.4017091607547,-12.9053495622083,-12.4089899636618,-11.9126303651153,
-11.4162707665689,-10.9199111680224,-10.4235515694759,-10.1495721867174),
 .UNSPECIFIED.);
#636=B_SPLINE_CURVE_WITH_KNOTS('',3,(#28805,#28806,#28807,#28808,#28809,
#28810,#28811,#28812,#28813,#28814,#28815,#28816,#28817,#28818,#28819,#28820,
#28821,#28822,#28823,#28824,#28825,#28826,#28827,#28828,#28829,#28830,#28831,
#28832,#28833,#28834,#28835,#28836,#28837,#28838,#28839,#28840,#28841,#28842,
#28843,#28844,#28845,#28846,#28847),.UNSPECIFIED.,.F.,.F.,(4,3,3,3,3,3,
3,3,3,3,3,3,3,3,4),(13.8754500755058,13.8980687593012,14.3944283578477,
14.8907879563942,15.3871475549406,15.8835071534871,16.3798667520336,16.87622635058,
17.3725859491265,17.868945547673,18.3653051462195,18.8616647447659,19.3580243433124,
19.8543839418589,20.1586353826853),.UNSPECIFIED.);
#637=B_SPLINE_CURVE_WITH_KNOTS('',3,(#28852,#28853,#28854,#28855,#28856,
#28857,#28858,#28859,#28860,#28861,#28862,#28863,#28864,#28865,#28866,#28867,
#28868,#28869,#28870,#28871,#28872,#28873,#28874,#28875,#28876,#28877,#28878,
#28879,#28880,#28881,#28882,#28883,#28884,#28885,#28886,#28887,#28888,#28889,
#28890,#28891),.UNSPECIFIED.,.F.,.F.,(4,3,3,3,3,3,3,3,3,3,3,3,3,4),(-22.7159428010765,
-22.3361819345912,-21.8398223360448,-21.3434627374983,-20.8471031389518,
-20.3507435404054,-19.8543839418589,-19.3580243433124,-18.8616647447659,
-18.3653051462195,-17.868945547673,-17.3725859491265,-16.8762263505801,
-16.432757493897),.UNSPECIFIED.);
#638=B_SPLINE_CURVE_WITH_KNOTS('',3,(#28892,#28893,#28894,#28895,#28896,
#28897,#28898,#28899,#28900,#28901,#28902,#28903,#28904,#28905,#28906,#28907,
#28908,#28909,#28910,#28911,#28912,#28913,#28914,#28915,#28916,#28917,#28918,
#28919,#28920,#28921,#28922,#28923,#28924,#28925,#28926,#28927,#28928,#28929,
#28930,#28931,#28932,#28933,#28934),.UNSPECIFIED.,.F.,.F.,(4,3,3,3,3,3,
3,3,3,3,3,3,3,3,4),(20.1586353826853,20.3507435404054,20.8471031389518,
21.3434627374983,21.8398223360448,22.3361819345912,22.8325415331377,23.3289011316842,
23.8252607302307,24.3216203287771,24.8179799273236,25.3143395258701,25.8106991244165,
26.307058722963,26.4418206898649),.UNSPECIFIED.);
#639=B_SPLINE_CURVE_WITH_KNOTS('',3,(#28939,#28940,#28941,#28942,#28943,
#28944,#28945,#28946,#28947,#28948,#28949,#28950,#28951,#28952,#28953,#28954,
#28955,#28956,#28957,#28958,#28959,#28960,#28961,#28962,#28963,#28964,#28965,
#28966,#28967,#28968,#28969,#28970,#28971,#28972,#28973,#28974,#28975,#28976,
#28977,#28978,#28979,#28980,#28981),.UNSPECIFIED.,.F.,.F.,(4,3,3,3,3,3,
3,3,3,3,3,3,3,3,4),(-28.9991281082561,-28.7888567156954,-28.2924971171489,
-27.7961375186024,-27.299777920056,-26.8034183215095,-26.307058722963,-25.8106991244165,
-25.3143395258701,-24.8179799273236,-24.3216203287771,-23.8252607302307,
-23.3289011316842,-22.8325415331377,-22.7159428010765),.UNSPECIFIED.);
#640=B_SPLINE_CURVE_WITH_KNOTS('',3,(#28982,#28983,#28984,#28985,#28986,
#28987,#28988,#28989,#28990,#28991,#28992,#28993,#28994,#28995,#28996,#28997,
#28998,#28999,#29000,#29001,#29002,#29003,#29004,#29005,#29006,#29007,#29008,
#29009,#29010,#29011,#29012,#29013,#29014,#29015,#29016,#29017,#29018,#29019,
#29020,#29021),.UNSPECIFIED.,.F.,.F.,(4,3,3,3,3,3,3,3,3,3,3,3,3,4),(26.4418206898649,
26.8034183215095,27.299777920056,27.7961375186024,28.2924971171489,28.7888567156954,
29.2852163142419,29.7815759127883,30.2779355113348,30.7742951098813,31.2706547084277,
31.7670143069742,32.2633739055207,32.7250059970445),.UNSPECIFIED.);
#641=B_SPLINE_CURVE_WITH_KNOTS('',3,(#29026,#29027,#29028,#29029,#29030,
#29031,#29032,#29033,#29034,#29035,#29036,#29037,#29038,#29039,#29040,#29041,
#29042,#29043,#29044,#29045,#29046,#29047,#29048,#29049,#29050,#29051,#29052,
#29053,#29054,#29055,#29056,#29057,#29058,#29059,#29060,#29061,#29062,#29063,
#29064,#29065,#29066,#29067,#29068),.UNSPECIFIED.,.F.,.F.,(4,3,3,3,3,3,
3,3,3,3,3,3,3,3,4),(-35.2823134154357,-35.2415314967995,-34.745171898253,
-34.2488122997066,-33.7524527011601,-33.2560931026136,-32.7597335040672,
-32.2633739055207,-31.7670143069742,-31.2706547084277,-30.7742951098813,
-30.2779355113348,-29.7815759127883,-29.2852163142419,-28.9991281082561),
 .UNSPECIFIED.);
#642=B_SPLINE_CURVE_WITH_KNOTS('',3,(#29069,#29070,#29071,#29072,#29073,
#29074,#29075,#29076,#29077,#29078,#29079,#29080,#29081,#29082,#29083,#29084,
#29085,#29086,#29087,#29088,#29089,#29090,#29091,#29092,#29093,#29094,#29095,
#29096,#29097,#29098,#29099,#29100,#29101,#29102,#29103,#29104,#29105,#29106,
#29107,#29108,#29109,#29110,#29111),.UNSPECIFIED.,.F.,.F.,(4,3,3,3,3,3,
3,3,3,3,3,3,3,3,4),(32.7250059970445,32.7597335040672,33.2560931026136,
33.7524527011601,34.2488122997066,34.7451718982531,35.2415314967995,35.737891095346,
36.2342506938925,36.7306102924389,37.2269698909854,37.7233294895319,38.2196890880783,
38.7160486866248,39.0081913042241),.UNSPECIFIED.);
#643=B_SPLINE_CURVE_WITH_KNOTS('',3,(#29116,#29117,#29118,#29119,#29120,
#29121,#29122,#29123,#29124,#29125,#29126,#29127,#29128,#29129,#29130,#29131,
#29132,#29133,#29134,#29135,#29136,#29137,#29138,#29139,#29140,#29141,#29142,
#29143,#29144,#29145,#29146,#29147,#29148,#29149,#29150,#29151,#29152,#29153,
#29154,#29155),.UNSPECIFIED.,.F.,.F.,(4,3,3,3,3,3,3,3,3,3,3,3,3,4),(-41.5654987226153,
-41.1978466793572,-40.7014870808107,-40.2051274822642,-39.7087678837178,
-39.2124082851713,-38.7160486866248,-38.2196890880784,-37.7233294895319,
-37.2269698909854,-36.7306102924389,-36.2342506938925,-35.737891095346,
-35.2823134154357),.UNSPECIFIED.);
#644=B_SPLINE_CURVE_WITH_KNOTS('',3,(#29156,#29157,#29158,#29159,#29160,
#29161,#29162,#29163,#29164,#29165,#29166,#29167,#29168,#29169,#29170,#29171,
#29172,#29173,#29174,#29175,#29176,#29177,#29178,#29179,#29180,#29181,#29182,
#29183,#29184,#29185,#29186,#29187,#29188,#29189,#29190,#29191,#29192,#29193,
#29194,#29195,#29196,#29197,#29198),.UNSPECIFIED.,.F.,.F.,(4,3,3,3,3,3,
3,3,3,3,3,3,3,3,4),(39.0081913042241,39.2124082851713,39.7087678837178,
40.2051274822642,40.7014870808107,41.1978466793572,41.6942062779036,42.1905658764501,
42.6869254749966,43.1832850735431,43.6796446720895,44.176004270636,44.6723638691825,
45.168723467729,45.2913766114037),.UNSPECIFIED.);
#645=B_SPLINE_CURVE_WITH_KNOTS('',3,(#29203,#29204,#29205,#29206,#29207,
#29208,#29209,#29210,#29211,#29212,#29213,#29214,#29215,#29216,#29217,#29218,
#29219,#29220,#29221,#29222,#29223,#29224,#29225,#29226,#29227,#29228,#29229,
#29230,#29231,#29232,#29233,#29234,#29235,#29236,#29237,#29238,#29239,#29240,
#29241,#29242,#29243,#29244,#29245),.UNSPECIFIED.,.F.,.F.,(4,3,3,3,3,3,
3,3,3,3,3,3,3,3,4),(-47.8486840297949,-47.6505214604613,-47.1541618619148,
-46.6578022633684,-46.1614426648219,-45.6650830662754,-45.168723467729,
-44.6723638691825,-44.176004270636,-43.6796446720895,-43.1832850735431,
-42.6869254749966,-42.1905658764501,-41.6942062779037,-41.5654987226153),
 .UNSPECIFIED.);
#646=B_SPLINE_CURVE_WITH_KNOTS('',3,(#29246,#29247,#29248,#29249,#29250,
#29251,#29252,#29253,#29254,#29255,#29256,#29257,#29258,#29259,#29260,#29261,
#29262,#29263,#29264,#29265,#29266,#29267,#29268,#29269,#29270,#29271,#29272,
#29273,#29274,#29275,#29276,#29277,#29278,#29279,#29280,#29281,#29282,#29283,
#29284,#29285),.UNSPECIFIED.,.F.,.F.,(4,3,3,3,3,3,3,3,3,3,3,3,3,4),(45.2913766114037,
45.6650830662754,46.1614426648219,46.6578022633684,47.1541618619148,47.6505214604613,
48.1468810590078,48.6432406575543,49.1396002561007,49.6359598546472,50.1323194531937,
50.6286790517402,51.1250386502866,51.5745619185833),.UNSPECIFIED.);
#647=B_SPLINE_CURVE_WITH_KNOTS('',3,(#29290,#29291,#29292,#29293,#29294,
#29295,#29296,#29297,#29298,#29299,#29300,#29301,#29302,#29303,#29304,#29305,
#29306,#29307,#29308,#29309,#29310,#29311,#29312,#29313,#29314,#29315,#29316,
#29317,#29318,#29319,#29320,#29321,#29322,#29323,#29324,#29325,#29326,#29327,
#29328,#29329,#29330,#29331,#29332),.UNSPECIFIED.,.F.,.F.,(4,3,3,3,3,3,
3,3,3,3,3,3,3,3,4),(-54.1318693369745,-54.1031962415655,-53.606836643019,
-53.1104770444725,-52.614117445926,-52.1177578473796,-51.6213982488331,
-51.1250386502866,-50.6286790517402,-50.1323194531937,-49.6359598546472,
-49.1396002561007,-48.6432406575543,-48.1468810590078,-47.8486840297949),
 .UNSPECIFIED.);
#648=B_SPLINE_CURVE_WITH_KNOTS('',3,(#29333,#29334,#29335,#29336,#29337,
#29338,#29339,#29340,#29341,#29342,#29343,#29344,#29345,#29346,#29347,#29348,
#29349,#29350,#29351,#29352,#29353,#29354,#29355,#29356,#29357,#29358,#29359,
#29360,#29361,#29362,#29363,#29364,#29365,#29366,#29367,#29368,#29369,#29370,
#29371,#29372,#29373,#29374,#29375),.UNSPECIFIED.,.F.,.F.,(4,3,3,3,3,3,
3,3,3,3,3,3,3,3,4),(51.5745619185833,51.6213982488331,52.1177578473796,
52.6141174459261,53.1104770444725,53.606836643019,54.1031962415655,54.5995558401119,
55.0959154386584,55.5922750372049,56.0886346357514,56.5849942342978,57.0813538328443,
57.5777134313908,57.8577472257629),.UNSPECIFIED.);
#649=B_SPLINE_CURVE_WITH_KNOTS('',3,(#29380,#29381,#29382,#29383,#29384,
#29385,#29386,#29387,#29388,#29389,#29390,#29391,#29392,#29393,#29394,#29395,
#29396,#29397,#29398,#29399,#29400,#29401,#29402,#29403,#29404,#29405,#29406,
#29407,#29408,#29409,#29410,#29411,#29412,#29413,#29414,#29415,#29416,#29417,
#29418,#29419),.UNSPECIFIED.,.F.,.F.,(4,3,3,3,3,3,3,3,3,3,3,3,3,4),(-60.4150546441541,
-60.0595114241231,-59.5631518255767,-59.0667922270302,-58.5704326284837,
-58.0740730299372,-57.5777134313908,-57.0813538328443,-56.5849942342978,
-56.0886346357513,-55.5922750372049,-55.0959154386584,-54.5995558401119,
-54.1318693369745),.UNSPECIFIED.);
#650=B_SPLINE_CURVE_WITH_KNOTS('',3,(#29420,#29421,#29422,#29423,#29424,
#29425,#29426,#29427,#29428,#29429,#29430,#29431,#29432,#29433,#29434,#29435,
#29436,#29437,#29438,#29439,#29440,#29441,#29442,#29443,#29444,#29445,#29446,
#29447,#29448,#29449,#29450,#29451,#29452,#29453,#29454,#29455,#29456,#29457,
#29458,#29459,#29460,#29461,#29462),.UNSPECIFIED.,.F.,.F.,(4,3,3,3,3,3,
3,3,3,3,3,3,3,3,4),(57.8577472257629,58.0740730299372,58.5704326284837,
59.0667922270302,59.5631518255767,60.0595114241231,60.5558710226696,61.0522306212161,
61.5485902197625,62.044949818309,62.5413094168555,63.037669015402,63.5340286139484,
64.0303882124949,64.1409325329425),.UNSPECIFIED.);
#651=B_SPLINE_CURVE_WITH_KNOTS('',3,(#29467,#29468,#29469,#29470,#29471,
#29472,#29473,#29474,#29475,#29476,#29477,#29478,#29479,#29480,#29481,#29482,
#29483,#29484,#29485,#29486,#29487,#29488,#29489,#29490,#29491,#29492,#29493,
#29494,#29495,#29496,#29497,#29498,#29499,#29500,#29501,#29502,#29503,#29504,
#29505,#29506,#29507,#29508,#29509),.UNSPECIFIED.,.F.,.F.,(4,3,3,3,3,3,
3,3,3,3,3,3,3,3,4),(-66.6982399513337,-66.5121862052273,-66.0158266066808,
-65.5194670081343,-65.0231074095879,-64.5267478110414,-64.0303882124949,
-63.5340286139484,-63.037669015402,-62.5413094168555,-62.044949818309,-61.5485902197625,
-61.0522306212161,-60.5558710226696,-60.4150546441541),.UNSPECIFIED.);
#652=B_SPLINE_CURVE_WITH_KNOTS('',3,(#29510,#29511,#29512,#29513,#29514,
#29515,#29516,#29517,#29518,#29519,#29520,#29521,#29522,#29523,#29524,#29525,
#29526,#29527,#29528,#29529,#29530,#29531,#29532,#29533,#29534,#29535,#29536,
#29537,#29538,#29539,#29540,#29541,#29542,#29543,#29544,#29545,#29546,#29547,
#29548,#29549),.UNSPECIFIED.,.F.,.F.,(4,3,3,3,3,3,3,3,3,3,3,3,3,4),(64.1409325329425,
64.5267478110414,65.0231074095878,65.5194670081343,66.0158266066808,66.5121862052273,
67.0085458037737,67.5049054023202,68.0012650008667,68.4976245994131,68.9939841979596,
69.4903437965061,69.9867033950526,70.4241178401221),.UNSPECIFIED.);
#653=B_SPLINE_CURVE_WITH_KNOTS('',3,(#29555,#29556,#29557,#29558,#29559,
#29560,#29561),.UNSPECIFIED.,.F.,.F.,(4,3,4),(76.7073031473017,76.9357377747032,
77.4320973732496),.UNSPECIFIED.);
#654=B_SPLINE_CURVE_WITH_KNOTS('',3,(#29564,#29565,#29566,#29567,#29568,
#29569,#29570,#29571,#29572,#29573,#29574,#29575,#29576,#29577,#29578,#29579),
 .UNSPECIFIED.,.F.,.F.,(4,3,3,3,3,4),(-75.398223686155,-74.9502993805173,
-74.4539397819708,-73.9575801834243,-73.4612205848779,-72.9814252585133),
 .UNSPECIFIED.);
#655=B_SPLINE_CURVE_WITH_KNOTS('',3,(#29585,#29586,#29587,#29588,#29589,
#29590,#29591,#29592,#29593,#29594,#29595,#29596),.UNSPECIFIED.,.F.,.F.,
(4,1,1,1,1,1,1,1,1,4),(84.8230016469244,85.302796973289,85.7991565718355,
86.295516170382,86.7918757689284,87.2882353674749,87.7845949660214,88.2809545645678,
88.7773141631143,89.2736737616608),.UNSPECIFIED.);
#656=B_SPLINE_CURVE_WITH_KNOTS('',3,(#29599,#29600,#29601,#29602,#29603,
#29604,#29605,#29606,#29607,#29608,#29609,#29610,#29611,#29612),
 .UNSPECIFIED.,.F.,.F.,(4,1,1,1,1,1,1,1,1,1,1,4),(84.8230016469244,84.8819468004013,
85.3783063989478,85.8746659974943,86.3710255960407,86.8673851945872,87.3637447931337,
87.8601043916802,88.3564639902266,88.8528235887731,89.3491831873196,89.7971074929573),
 .UNSPECIFIED.);
#657=B_SPLINE_CURVE_WITH_KNOTS('',3,(#29617,#29618,#29619,#29620,#29621,
#29622,#29623,#29624,#29625,#29626,#29627,#29628,#29629,#29630,#29631,#29632,
#29633),.UNSPECIFIED.,.F.,.F.,(4,1,1,1,1,1,1,1,1,1,1,1,1,1,4),(78.5398163397448,
78.8501221921849,79.3464817907313,79.8428413892778,80.3392009878243,80.8355605863708,
81.3319201849172,81.8282797834637,82.3246393820102,82.8209989805567,83.3173585791031,
83.8137181776496,84.3100777761961,84.8064373747425,84.8230016469244),
 .UNSPECIFIED.);
#658=B_SPLINE_CURVE_WITH_KNOTS('',3,(#29634,#29635,#29636,#29637,#29638,
#29639,#29640,#29641,#29642,#29643,#29644,#29645,#29646,#29647,#29648,#29649),
 .UNSPECIFIED.,.F.,.F.,(4,1,1,1,1,1,1,1,1,1,1,1,1,4),(78.5398163397448,
78.9256316178437,79.4219912163901,79.9183508149366,80.4147104134831,80.9110700120296,
81.407429610576,81.9037892091225,82.400148807669,82.8965084062154,83.3928680047619,
83.8892276033084,84.3855872018549,84.8230016469244),.UNSPECIFIED.);
#659=B_SPLINE_CURVE_WITH_KNOTS('',3,(#29654,#29655,#29656,#29657,#29658,
#29659,#29660,#29661,#29662,#29663,#29664,#29665,#29666,#29667,#29668,#29669,
#29670),.UNSPECIFIED.,.F.,.F.,(4,1,1,1,1,1,1,1,1,1,1,1,1,1,4),(72.2566310325652,
72.3974474110807,72.8938070096272,73.3901666081737,73.8865262067201,74.3828858052666,
74.8792454038131,75.3756050023596,75.871964600906,76.3683241994525,76.864683797999,
77.3610433965455,77.8574029950919,78.3537625936384,78.5398163397448),
 .UNSPECIFIED.);
#660=B_SPLINE_CURVE_WITH_KNOTS('',3,(#29671,#29672,#29673,#29674,#29675,
#29676,#29677,#29678,#29679,#29680,#29681,#29682,#29683,#29684,#29685,#29686,
#29687),.UNSPECIFIED.,.F.,.F.,(4,1,1,1,1,1,1,1,1,1,1,1,1,1,4),(72.2566310325652,
72.4729568367395,72.969316435286,73.4656760338325,73.9620356323789,74.4583952309254,
74.9547548294719,75.4511144280183,75.9474740265648,76.4438336251113,76.9401932236578,
77.4365528222042,77.9329124207507,78.4292720192972,78.5398163397448),
 .UNSPECIFIED.);
#661=B_SPLINE_CURVE_WITH_KNOTS('',3,(#29692,#29693,#29694,#29695,#29696,
#29697,#29698,#29699,#29700,#29701,#29702,#29703,#29704,#29705,#29706,#29707),
 .UNSPECIFIED.,.F.,.F.,(4,1,1,1,1,1,1,1,1,1,1,1,1,4),(65.9734457253856,
66.4411322285231,66.9374918270696,67.433851425616,67.9302110241625,68.426570622709,
68.9229302212554,69.4192898198019,69.9156494183484,70.4120090168948,70.9083686154413,
71.4047282139878,71.9010878125343,72.2566310325652),.UNSPECIFIED.);
#662=B_SPLINE_CURVE_WITH_KNOTS('',3,(#29708,#29709,#29710,#29711,#29712,
#29713,#29714,#29715,#29716,#29717,#29718,#29719,#29720,#29721,#29722,#29723,
#29724),.UNSPECIFIED.,.F.,.F.,(4,1,1,1,1,1,1,1,1,1,1,1,1,1,4),(65.9734457253856,
66.0202820556354,66.5166416541819,67.0130012527283,67.5093608512748,68.0057204498213,
68.5020800483677,68.9984396469142,69.4947992454607,69.9911588440072,70.4875184425536,
70.9838780411001,71.4802376396466,71.9765972381931,72.2566310325652),
 .UNSPECIFIED.);
#663=B_SPLINE_CURVE_WITH_KNOTS('',3,(#29729,#29730,#29731,#29732,#29733,
#29734,#29735,#29736,#29737,#29738,#29739,#29740,#29741,#29742,#29743,#29744,
#29745),.UNSPECIFIED.,.F.,.F.,(4,1,1,1,1,1,1,1,1,1,1,1,1,1,4),(59.690260418206,
59.9884574474189,60.4848170459654,60.9811766445119,61.4775362430584,61.9738958416048,
62.4702554401513,62.9666150386978,63.4629746372442,63.9593342357907,64.4556938343372,
64.9520534328837,65.4484130314301,65.9447726299766,65.9734457253856),
 .UNSPECIFIED.);
#664=B_SPLINE_CURVE_WITH_KNOTS('',3,(#29746,#29747,#29748,#29749,#29750,
#29751,#29752,#29753,#29754,#29755,#29756,#29757,#29758,#29759,#29760,#29761),
 .UNSPECIFIED.,.F.,.F.,(4,1,1,1,1,1,1,1,1,1,1,1,1,4),(59.690260418206,60.0639668730777,
60.5603264716242,61.0566860701707,61.5530456687171,62.0494052672636,62.5457648658101,
63.0421244643565,63.538484062903,64.0348436614495,64.531203259996,65.0275628585424,
65.5239224570889,65.9734457253856),.UNSPECIFIED.);
#665=B_SPLINE_CURVE_WITH_KNOTS('',3,(#29766,#29767,#29768,#29769,#29770,
#29771,#29772,#29773,#29774,#29775,#29776,#29777,#29778,#29779,#29780,#29781,
#29782),.UNSPECIFIED.,.F.,.F.,(4,1,1,1,1,1,1,1,1,1,1,1,1,1,4),(53.4070751110265,
53.5357826663148,54.0321422648613,54.5285018634077,55.0248614619542,55.5212210605007,
56.0175806590472,56.5139402575936,57.0102998561401,57.5066594546866,58.003019053233,
58.4993786517795,58.995738250326,59.4920978488725,59.690260418206),
 .UNSPECIFIED.);
#666=B_SPLINE_CURVE_WITH_KNOTS('',3,(#29783,#29784,#29785,#29786,#29787,
#29788,#29789,#29790,#29791,#29792,#29793,#29794,#29795,#29796,#29797,#29798,
#29799),.UNSPECIFIED.,.F.,.F.,(4,1,1,1,1,1,1,1,1,1,1,1,1,1,4),(53.4070751110264,
53.6112920919736,54.1076516905201,54.6040112890665,55.100370887613,55.5967304861595,
56.0930900847059,56.5894496832524,57.0858092817989,57.5821688803454,58.0785284788918,
58.5748880774383,59.0712476759848,59.5676072745312,59.690260418206),
 .UNSPECIFIED.);
#667=B_SPLINE_CURVE_WITH_KNOTS('',3,(#29804,#29805,#29806,#29807,#29808,
#29809,#29810,#29811,#29812,#29813,#29814,#29815,#29816,#29817,#29818,#29819),
 .UNSPECIFIED.,.F.,.F.,(4,1,1,1,1,1,1,1,1,1,1,1,1,4),(47.1238898038468,
47.5794674837571,48.0758270823036,48.5721866808501,49.0685462793965,49.564905877943,
50.0612654764895,50.557625075036,51.0539846735824,51.5503442721289,52.0467038706754,
52.5430634692219,53.0394230677683,53.4070751110265),.UNSPECIFIED.);
#668=B_SPLINE_CURVE_WITH_KNOTS('',3,(#29820,#29821,#29822,#29823,#29824,
#29825,#29826,#29827,#29828,#29829,#29830,#29831,#29832,#29833,#29834,#29835,
#29836),.UNSPECIFIED.,.F.,.F.,(4,1,1,1,1,1,1,1,1,1,1,1,1,1,4),(47.1238898038469,
47.1586173108694,47.6549769094159,48.1513365079624,48.6476961065089,49.1440557050553,
49.6404153036018,50.1367749021483,50.6331345006947,51.1294940992412,51.6258536977877,
52.1222132963342,52.6185728948806,53.1149324934271,53.4070751110264),
 .UNSPECIFIED.);
#669=B_SPLINE_CURVE_WITH_KNOTS('',3,(#29841,#29842,#29843,#29844,#29845,
#29846,#29847,#29848,#29849,#29850,#29851,#29852,#29853,#29854,#29855,#29856,
#29857),.UNSPECIFIED.,.F.,.F.,(4,1,1,1,1,1,1,1,1,1,1,1,1,1,4),(40.8407044966672,
41.126792702653,41.6231523011995,42.1195118997459,42.6158714982924,43.1122310968389,
43.6085906953854,44.1049502939318,44.6013098924783,45.0976694910248,45.5940290895712,
46.0903886881177,46.5867482866642,47.0831078852107,47.1238898038468),
 .UNSPECIFIED.);
#670=B_SPLINE_CURVE_WITH_KNOTS('',3,(#29858,#29859,#29860,#29861,#29862,
#29863,#29864,#29865,#29866,#29867,#29868,#29869,#29870,#29871,#29872,#29873),
 .UNSPECIFIED.,.F.,.F.,(4,1,1,1,1,1,1,1,1,1,1,1,1,4),(40.8407044966673,
41.2023021283118,41.6986617268582,42.1950213254047,42.6913809239512,43.1877405224977,
43.6841001210441,44.1804597195906,44.6768193181371,45.1731789166836,45.66953851523,
46.1658981137765,46.662257712323,47.1238898038469),.UNSPECIFIED.);
#671=B_SPLINE_CURVE_WITH_KNOTS('',3,(#29878,#29879,#29880,#29881,#29882,
#29883,#29884,#29885,#29886,#29887,#29888,#29889,#29890,#29891,#29892,#29893,
#29894),.UNSPECIFIED.,.F.,.F.,(4,1,1,1,1,1,1,1,1,1,1,1,1,1,4),(34.5575191894877,
34.6741179215489,35.1704775200953,35.6668371186418,36.1631967171883,36.6595563157347,
37.1559159142812,37.6522755128277,38.1486351113742,38.6449947099206,39.1413543084671,
39.6377139070136,40.1340735055601,40.6304331041065,40.8407044966672),
 .UNSPECIFIED.);
#672=B_SPLINE_CURVE_WITH_KNOTS('',3,(#29895,#29896,#29897,#29898,#29899,
#29900,#29901,#29902,#29903,#29904,#29905,#29906,#29907,#29908,#29909,#29910,
#29911),.UNSPECIFIED.,.F.,.F.,(4,1,1,1,1,1,1,1,1,1,1,1,1,1,4),(34.5575191894877,
34.7496273472076,35.2459869457541,35.7423465443006,36.2387061428471,36.7350657413935,
37.23142533994,37.7277849384865,38.2241445370329,38.7205041355794,39.2168637341259,
39.7132233326724,40.2095829312188,40.7059425297653,40.8407044966673),
 .UNSPECIFIED.);
#673=B_SPLINE_CURVE_WITH_KNOTS('',3,(#29916,#29917,#29918,#29919,#29920,
#29921,#29922,#29923,#29924,#29925,#29926,#29927,#29928,#29929,#29930,#29931),
 .UNSPECIFIED.,.F.,.F.,(4,1,1,1,1,1,1,1,1,1,1,1,1,4),(28.2743338823081,
28.7178027389912,29.2141623375377,29.7105219360841,30.2068815346306,30.7032411331771,
31.1996007317236,31.69596033027,32.1923199288165,32.688679527363,33.1850391259094,
33.6813987244559,34.1777583230024,34.5575191894877),.UNSPECIFIED.);
#674=B_SPLINE_CURVE_WITH_KNOTS('',3,(#29932,#29933,#29934,#29935,#29936,
#29937,#29938,#29939,#29940,#29941,#29942,#29943,#29944,#29945,#29946,#29947,
#29948),.UNSPECIFIED.,.F.,.F.,(4,1,1,1,1,1,1,1,1,1,1,1,1,1,4),(28.2743338823081,
28.2969525661035,28.79331216465,29.2896717631964,29.7860313617429,30.2823909602894,
30.7787505588359,31.2751101573823,31.7714697559288,32.2678293544753,32.7641889530218,
33.2605485515682,33.7569081501147,34.2532677486612,34.5575191894877),
 .UNSPECIFIED.);
#675=B_SPLINE_CURVE_WITH_KNOTS('',3,(#29953,#29954,#29955,#29956,#29957,
#29958,#29959,#29960,#29961,#29962,#29963,#29964,#29965,#29966,#29967,#29968,
#29969),.UNSPECIFIED.,.F.,.F.,(4,1,1,1,1,1,1,1,1,1,1,1,1,1,4),(21.9911485751285,
22.2651279578871,22.7614875564335,23.25784715498,23.7542067535265,24.2505663520729,
24.7469259506194,25.2432855491659,25.7396451477124,26.2360047462588,26.7323643448053,
27.2287239433518,27.7250835418983,28.2214431404447,28.2743338823081),
 .UNSPECIFIED.);
#676=B_SPLINE_CURVE_WITH_KNOTS('',3,(#29970,#29971,#29972,#29973,#29974,
#29975,#29976,#29977,#29978,#29979,#29980,#29981,#29982,#29983,#29984,#29985),
 .UNSPECIFIED.,.F.,.F.,(4,1,1,1,1,1,1,1,1,1,1,1,1,4),(21.9911485751285,
22.3406373835458,22.8369969820923,23.3333565806388,23.8297161791853,24.3260757777317,
24.8224353762782,25.3187949748247,25.8151545733711,26.3115141719176,26.8078737704641,
27.3042333690106,27.800592967557,28.2743338823081),.UNSPECIFIED.);
#677=B_SPLINE_CURVE_WITH_KNOTS('',3,(#29991,#29992,#29993,#29994,#29995,
#29996),.UNSPECIFIED.,.F.,.F.,(4,1,1,4),(14.3988838068023,14.8952434053488,
15.3916030038952,15.7079632679489),.UNSPECIFIED.);
#678=B_SPLINE_CURVE_WITH_KNOTS('',3,(#29999,#30000,#30001,#30002,#30003,
#30004,#30005),.UNSPECIFIED.,.F.,.F.,(4,1,1,1,4),(13.8754500755058,14.3233743811435,
14.81973397969,15.3160935782364,15.7079632679489),.UNSPECIFIED.);
#679=B_SPLINE_CURVE_WITH_KNOTS('',3,(#30007,#30008,#30009,#30010,#30011,
#30012,#30013,#30014,#30015,#30016,#30017,#30018,#30019,#30020,#30021,#30022,
#30023),.UNSPECIFIED.,.F.,.F.,(4,1,1,1,1,1,1,1,1,1,1,1,1,1,4),(15.7079632679489,
15.8124531767829,16.3088127753294,16.8051723738759,17.3015319724223,17.7978915709688,
18.2942511695153,18.7906107680618,19.2869703666082,19.7833299651547,20.2796895637012,
20.7760491622476,21.2724087607941,21.7687683593406,21.9911485751285),
 .UNSPECIFIED.);
#680=B_SPLINE_CURVE_WITH_KNOTS('',3,(#30024,#30025,#30026,#30027,#30028,
#30029,#30030,#30031,#30032,#30033,#30034,#30035,#30036,#30037,#30038,#30039,
#30040),.UNSPECIFIED.,.F.,.F.,(4,1,1,1,1,1,1,1,1,1,1,1,1,1,4),(15.7079632679489,
15.8879626024417,16.3843222009882,16.8806817995346,17.3770413980811,17.8734009966276,
18.3697605951741,18.8661201937205,19.362479792267,19.8588393908135,20.3551989893599,
20.8515585879064,21.3479181864529,21.8442777849994,21.9911485751285),
 .UNSPECIFIED.);
#681=B_SPLINE_CURVE_WITH_KNOTS('',3,(#30677,#30678,#30679,#30680,#30681,
#30682,#30683,#30684,#30685,#30686,#30687,#30688,#30689,#30690,#30691,#30692,
#30693,#30694,#30695,#30696,#30697,#30698,#30699,#30700,#30701,#30702,#30703,
#30704,#30705,#30706,#30707,#30708,#30709,#30710,#30711,#30712,#30713,#30714,
#30715,#30716,#30717,#30718,#30719,#30720,#30721,#30722,#30723,#30724,#30725,
#30726,#30727,#30728,#30729,#30730,#30731,#30732,#30733,#30734,#30735,#30736,
#30737,#30738,#30739,#30740,#30741,#30742,#30743,#30744,#30745,#30746,#30747,
#30748,#30749,#30750,#30751,#30752,#30753,#30754,#30755,#30756,#30757,#30758,
#30759,#30760,#30761,#30762,#30763,#30764,#30765,#30766,#30767,#30768,#30769,
#30770,#30771,#30772,#30773,#30774,#30775,#30776,#30777,#30778,#30779,#30780,
#30781,#30782,#30783,#30784,#30785,#30786,#30787,#30788,#30789,#30790,#30791,
#30792,#30793,#30794),.UNSPECIFIED.,.F.,.F.,(4,3,3,3,3,3,3,3,3,3,3,3,3,
3,3,3,3,3,3,3,3,3,3,3,3,3,3,3,3,3,3,3,3,3,3,3,3,3,3,4),(0.,0.0741055703209817,
0.149042386837593,0.22431310048934,0.299024282623367,0.348898308601355,
0.386899824489537,0.397140150473765,0.471842661155879,0.498520386535318,
0.573008003563107,0.64782102937255,0.722388891944134,0.756126730638512,
0.773706375489234,0.785503175786165,0.859722753314182,0.93387483248313,
0.992291601499154,1.0666323863286,1.11842843879762,1.14419898358481,1.16194416695704,
1.17045593848397,1.24384647704758,1.31776148692053,1.39143934948928,1.46416752858594,
1.48100080608073,1.54133664964938,1.55357748542717,1.62672847250257,1.70016992001151,
1.76604932866612,1.77729599120305,1.78733100079922,1.86043957741219,1.93296531556185,
1.96368755462996,2.01048691722679),.UNSPECIFIED.);
#682=B_SPLINE_CURVE_WITH_KNOTS('',3,(#30795,#30796,#30797,#30798,#30799,
#30800,#30801,#30802,#30803,#30804,#30805,#30806,#30807,#30808,#30809,#30810,
#30811,#30812,#30813,#30814,#30815,#30816,#30817,#30818,#30819,#30820,#30821,
#30822,#30823,#30824,#30825,#30826,#30827,#30828,#30829,#30830,#30831,#30832,
#30833,#30834,#30835,#30836,#30837,#30838,#30839,#30840,#30841,#30842,#30843,
#30844,#30845,#30846,#30847,#30848,#30849,#30850,#30851,#30852,#30853,#30854,
#30855,#30856,#30857,#30858,#30859,#30860,#30861,#30862,#30863,#30864,#30865,
#30866,#30867,#30868,#30869,#30870,#30871,#30872,#30873,#30874,#30875,#30876,
#30877,#30878,#30879,#30880,#30881,#30882,#30883,#30884,#30885,#30886,#30887,
#30888,#30889,#30890,#30891,#30892,#30893,#30894,#30895,#30896,#30897,#30898,
#30899,#30900,#30901,#30902,#30903,#30904,#30905,#30906,#30907,#30908,#30909,
#30910,#30911,#30912,#30913,#30914,#30915),.UNSPECIFIED.,.F.,.F.,(4,3,3,
3,3,3,3,3,3,3,3,3,3,3,3,3,3,3,3,3,3,3,3,3,3,3,3,3,3,3,3,3,3,3,3,3,3,3,3,
3,4),(0.,0.0717333891578521,0.144434524784762,0.217681915638706,0.290732086867526,
0.338695801228598,0.3585952673969,0.371352699087487,0.37922575171661,0.452863071133944,
0.482586944311812,0.555696925706304,0.629354906824166,0.703026073008598,
0.736450321070254,0.753797084226665,0.764865100699128,0.838737800631782,
0.912894416882333,0.970420057501849,1.04449202061033,1.09683033801563,1.12306068482966,
1.14298639667138,1.15119020265998,1.22496157430685,1.29957989448712,1.37416452133182,
1.44802364319018,1.46319855985276,1.52529555501938,1.53710295111153,1.61136302920978,
1.68616208034702,1.7546151905567,1.76661170976244,1.77674419461876,1.85186181207957,
1.92670088998344,1.95997452118572,2.00868916811693),.UNSPECIFIED.);
#683=B_SPLINE_CURVE_WITH_KNOTS('',3,(#30916,#30917,#30918,#30919,#30920,
#30921,#30922,#30923,#30924,#30925,#30926,#30927,#30928,#30929,#30930,#30931,
#30932,#30933,#30934,#30935,#30936,#30937,#30938,#30939,#30940,#30941,#30942,
#30943,#30944,#30945,#30946,#30947,#30948,#30949,#30950,#30951,#30952,#30953,
#30954,#30955,#30956,#30957,#30958),.UNSPECIFIED.,.F.,.F.,(4,3,3,3,3,3,
3,3,3,3,3,3,3,3,4),(-72.9814252585133,-72.9648609863314,-72.4685013877849,
-71.9721417892385,-71.475782190692,-70.9794225921455,-70.483062993599,-69.9867033950526,
-69.4903437965061,-68.9939841979596,-68.4976245994131,-68.0012650008667,
-67.5049054023202,-67.0085458037737,-66.6982399513337),.UNSPECIFIED.);
#684=B_SPLINE_CURVE_WITH_KNOTS('',3,(#31595,#31596,#31597,#31598,#31599,
#31600,#31601,#31602,#31603,#31604,#31605,#31606,#31607,#31608,#31609,#31610,
#31611,#31612,#31613,#31614,#31615,#31616,#31617,#31618,#31619,#31620,#31621,
#31622,#31623,#31624,#31625,#31626,#31627,#31628,#31629,#31630,#31631,#31632,
#31633,#31634,#31635,#31636,#31637,#31638,#31639,#31640,#31641,#31642,#31643,
#31644,#31645,#31646,#31647,#31648,#31649,#31650,#31651,#31652,#31653,#31654,
#31655,#31656,#31657,#31658,#31659,#31660,#31661,#31662,#31663,#31664,#31665,
#31666,#31667,#31668,#31669,#31670,#31671,#31672,#31673,#31674,#31675,#31676,
#31677,#31678,#31679,#31680,#31681,#31682,#31683,#31684,#31685,#31686,#31687,
#31688,#31689,#31690,#31691,#31692,#31693,#31694,#31695,#31696,#31697,#31698,
#31699,#31700,#31701,#31702,#31703,#31704,#31705,#31706,#31707,#31708,#31709,
#31710,#31711,#31712,#31713,#31714,#31715),.UNSPECIFIED.,.F.,.F.,(4,3,3,
3,3,3,3,3,3,3,3,3,3,3,3,3,3,3,3,3,3,3,3,3,3,3,3,3,3,3,3,3,3,3,3,3,3,3,3,
3,4),(0.,0.0717334165710816,0.14443457078409,0.217681968816114,0.290732129582985,
0.338695833265186,0.358595323769131,0.371352811334654,0.379225821480966,
0.452863145034527,0.482586944311789,0.555696909117683,0.629354883241453,
0.703026051028594,0.736450301837749,0.75379706834374,0.764865101436399,
0.838737791296975,0.91289440941722,0.970420057501839,1.044492023981,1.09683034096497,
1.1230606915887,1.14298630277634,1.15119019060978,1.2249615711206,1.29957989345465,
1.37416452034083,1.44802364240076,1.46319855985276,1.52529555501938,1.53710295132795,
1.61136302929257,1.68616208097367,1.75461519102668,1.7666117106576,1.77674419560174,
1.85186181352304,1.9267008900023,1.95997452118571,2.00868916811694),
 .UNSPECIFIED.);
#685=B_SPLINE_CURVE_WITH_KNOTS('',3,(#31716,#31717,#31718,#31719,#31720,
#31721,#31722,#31723,#31724,#31725,#31726,#31727,#31728,#31729,#31730,#31731,
#31732,#31733,#31734,#31735,#31736,#31737,#31738,#31739,#31740,#31741,#31742,
#31743,#31744,#31745,#31746,#31747,#31748,#31749,#31750,#31751,#31752,#31753,
#31754,#31755,#31756,#31757,#31758),.UNSPECIFIED.,.F.,.F.,(4,3,3,3,3,3,
3,3,3,3,3,3,3,3,4),(70.4241178401221,70.483062993599,70.9794225921455,71.475782190692,
71.9721417892384,72.4685013877849,72.9648609863314,73.4612205848779,73.9575801834243,
74.4539397819708,74.9502993805173,75.4466589790638,75.9430185776102,76.4393781761567,
76.7073031473017),.UNSPECIFIED.);
#686=B_SPLINE_CURVE_WITH_KNOTS('',3,(#31759,#31760,#31761,#31762,#31763,
#31764,#31765,#31766,#31767,#31768,#31769,#31770,#31771,#31772,#31773,#31774,
#31775,#31776,#31777,#31778,#31779,#31780,#31781,#31782,#31783,#31784,#31785,
#31786,#31787,#31788,#31789,#31790,#31791,#31792,#31793,#31794,#31795,#31796,
#31797,#31798,#31799,#31800,#31801,#31802,#31803,#31804,#31805,#31806,#31807,
#31808,#31809,#31810,#31811,#31812,#31813,#31814,#31815,#31816,#31817,#31818,
#31819,#31820,#31821,#31822,#31823,#31824,#31825,#31826,#31827,#31828,#31829,
#31830,#31831,#31832,#31833,#31834,#31835,#31836,#31837,#31838,#31839,#31840,
#31841,#31842,#31843,#31844,#31845,#31846,#31847,#31848,#31849,#31850,#31851,
#31852,#31853,#31854,#31855,#31856,#31857,#31858,#31859,#31860,#31861,#31862,
#31863,#31864,#31865,#31866,#31867,#31868,#31869,#31870,#31871,#31872,#31873,
#31874,#31875,#31876),.UNSPECIFIED.,.F.,.F.,(4,3,3,3,3,3,3,3,3,3,3,3,3,
3,3,3,3,3,3,3,3,3,3,3,3,3,3,3,3,3,3,3,3,3,3,3,3,3,3,4),(0.,0.0741055943583196,
0.149042424272304,0.224313139225513,0.299024306861181,0.348898326779717,
0.3868998616391,0.397140157099964,0.471842665351292,0.498520386535326,0.573007992260638,
0.647821015783437,0.722388882730898,0.756126722576926,0.773706368904776,
0.78550317616495,0.859722748844764,0.93387483251693,0.992291601499126,1.06663238757372,
1.1184284398871,1.1441989874156,1.16194405544069,1.17045593148218,1.24384647547351,
1.31776148594777,1.39143934859838,1.46416752984131,1.48100080608075,1.5413366496494,
1.55357748570526,1.62672847367446,1.70016992167766,1.76604932991573,1.77729599482936,
1.78733100568737,1.86043958226664,1.93296531739482,1.96368755462995,2.01048691722678),
 .UNSPECIFIED.);
#687=B_SPLINE_CURVE_WITH_KNOTS('',3,(#31903,#31904,#31905,#31906,#31907,
#31908,#31909,#31910,#31911,#31912),.UNSPECIFIED.,.F.,.F.,(4,3,3,4),(-4.09293042013066,
-3.91533412349299,-2.93650059261974,-2.06863817490914),.UNSPECIFIED.);
#688=B_SPLINE_CURVE_WITH_KNOTS('',3,(#31915,#31916,#31917,#31918,#31919,
#31920,#31921),.UNSPECIFIED.,.F.,.F.,(4,3,4),(0.,0.978833530873248,1.11730040836829),
 .UNSPECIFIED.);
#689=B_SPLINE_CURVE_WITH_KNOTS('',3,(#31926,#31927,#31928,#31929,#31930,
#31931,#31932,#31933,#31934,#31935,#31936,#31937,#31938,#31939,#31940,#31941,
#31942,#31943,#31944,#31945,#31946,#31947),.UNSPECIFIED.,.F.,.F.,(4,3,3,
3,3,3,3,4),(-10.3761157273103,-9.78833530873246,-8.80950177785921,-7.83066824698597,
-6.85183471611273,-5.87300118523948,-4.89416765436623,-4.09293042013066),
 .UNSPECIFIED.);
#690=B_SPLINE_CURVE_WITH_KNOTS('',3,(#31948,#31949,#31950,#31951,#31952,
#31953,#31954,#31955,#31956,#31957,#31958,#31959,#31960,#31961,#31962,#31963,
#31964,#31965,#31966,#31967,#31968,#31969),.UNSPECIFIED.,.F.,.F.,(4,3,3,
3,3,3,3,4),(1.11730040836829,1.95766706174649,2.93650059261974,3.91533412349299,
4.89416765436624,5.87300118523948,6.85183471611273,7.40048571554788),
 .UNSPECIFIED.);
#691=B_SPLINE_CURVE_WITH_KNOTS('',3,(#31974,#31975,#31976,#31977,#31978,
#31979,#31980,#31981,#31982,#31983,#31984,#31985,#31986,#31987,#31988,#31989,
#31990,#31991,#31992,#31993,#31994,#31995,#31996,#31997,#31998),
 .UNSPECIFIED.,.F.,.F.,(4,3,3,3,3,3,3,3,4),(-16.6593010344898,-16.6401700248452,
-15.6613364939719,-14.6825029630987,-13.7036694322255,-12.7248359013522,
-11.746002370479,-10.7671688396057,-10.3761157273103),.UNSPECIFIED.);
#692=B_SPLINE_CURVE_WITH_KNOTS('',3,(#31999,#32000,#32001,#32002,#32003,
#32004,#32005,#32006,#32007,#32008,#32009,#32010,#32011,#32012,#32013,#32014,
#32015,#32016,#32017,#32018,#32019,#32020),.UNSPECIFIED.,.F.,.F.,(4,3,3,
3,3,3,3,4),(7.40048571554788,7.83066824698597,8.80950177785922,9.78833530873247,
10.7671688396057,11.746002370479,12.7248359013522,13.6836710227275),
 .UNSPECIFIED.);
#693=B_SPLINE_CURVE_WITH_KNOTS('',3,(#32025,#32026,#32027,#32028,#32029,
#32030,#32031,#32032,#32033,#32034,#32035,#32036,#32037,#32038,#32039,#32040,
#32041,#32042,#32043,#32044,#32045,#32046),.UNSPECIFIED.,.F.,.F.,(4,3,3,
3,3,3,3,4),(-22.9424863416694,-22.5131712100847,-21.5343376792114,-20.5555041483382,
-19.5766706174649,-18.5978370865917,-17.6190035557184,-16.6593010344898),
 .UNSPECIFIED.);
#694=B_SPLINE_CURVE_WITH_KNOTS('',3,(#32047,#32048,#32049,#32050,#32051,
#32052,#32053,#32054,#32055,#32056,#32057,#32058,#32059,#32060,#32061,#32062,
#32063,#32064,#32065,#32066,#32067,#32068,#32069,#32070,#32071),
 .UNSPECIFIED.,.F.,.F.,(4,3,3,3,3,3,3,3,4),(13.6836710227275,13.7036694322254,
14.6825029630987,15.6613364939719,16.6401700248452,17.6190035557184,18.5978370865917,
19.5766706174649,19.966856329907),.UNSPECIFIED.);
#695=B_SPLINE_CURVE_WITH_KNOTS('',3,(#32076,#32077,#32078,#32079,#32080,
#32081,#32082,#32083,#32084,#32085,#32086,#32087,#32088,#32089,#32090,#32091,
#32092,#32093,#32094,#32095,#32096,#32097),.UNSPECIFIED.,.F.,.F.,(4,3,3,
3,3,3,3,4),(-29.225671648849,-28.3861723953241,-27.4073388644509,-26.4285053335777,
-25.4496718027044,-24.4708382718312,-23.4920047409579,-22.9424863416694),
 .UNSPECIFIED.);
#696=B_SPLINE_CURVE_WITH_KNOTS('',3,(#32098,#32099,#32100,#32101,#32102,
#32103,#32104,#32105,#32106,#32107,#32108,#32109,#32110,#32111,#32112,#32113,
#32114,#32115,#32116,#32117,#32118,#32119),.UNSPECIFIED.,.F.,.F.,(4,3,3,
3,3,3,3,4),(19.966856329907,20.5555041483382,21.5343376792114,22.5131712100847,
23.4920047409579,24.4708382718312,25.4496718027044,26.2500416370866),
 .UNSPECIFIED.);
#697=B_SPLINE_CURVE_WITH_KNOTS('',3,(#32124,#32125,#32126,#32127,#32128,
#32129,#32130,#32131,#32132,#32133,#32134,#32135,#32136,#32137,#32138,#32139,
#32140,#32141,#32142,#32143,#32144,#32145,#32146,#32147,#32148),
 .UNSPECIFIED.,.F.,.F.,(4,3,3,3,3,3,3,3,4),(-35.5088569560286,-35.2380071114369,
-34.2591735805636,-33.2803400496904,-32.3015065188171,-31.3226729879439,
-30.3438394570706,-29.3650059261974,-29.225671648849),.UNSPECIFIED.);
#698=B_SPLINE_CURVE_WITH_KNOTS('',3,(#32149,#32150,#32151,#32152,#32153,
#32154,#32155,#32156,#32157,#32158,#32159,#32160,#32161,#32162,#32163,#32164,
#32165,#32166,#32167,#32168,#32169,#32170,#32171,#32172,#32173),
 .UNSPECIFIED.,.F.,.F.,(4,3,3,3,3,3,3,3,4),(26.2500416370866,26.4285053335777,
27.4073388644509,28.3861723953241,29.3650059261974,30.3438394570707,31.3226729879439,
32.3015065188171,32.5332269442662),.UNSPECIFIED.);
#699=B_SPLINE_CURVE_WITH_KNOTS('',3,(#32179,#32180,#32181,#32182,#32183,
#32184),.UNSPECIFIED.,.F.,.F.,(4,1,1,4),(47.1238898038469,47.8318734901284,
48.8107070210017,49.6785694387123),.UNSPECIFIED.);
#700=B_SPLINE_CURVE_WITH_KNOTS('',3,(#32187,#32188,#32189,#32190,#32191),
 .UNSPECIFIED.,.F.,.F.,(4,1,4),(47.1238898038469,47.460818787331,48.4396523182042),
 .UNSPECIFIED.);
#701=B_SPLINE_CURVE_WITH_KNOTS('',3,(#32196,#32197,#32198,#32199,#32200,
#32201,#32202,#32203,#32204,#32205,#32206),.UNSPECIFIED.,.F.,.F.,(4,1,1,
1,1,1,1,1,4),(40.8407044966673,40.9800387740157,41.9588723048889,42.9377058357622,
43.9165393666354,44.8953728975087,45.8742064283819,46.8530399592552,47.1238898038469),
 .UNSPECIFIED.);
#702=B_SPLINE_CURVE_WITH_KNOTS('',3,(#32207,#32208,#32209,#32210,#32211,
#32212,#32213,#32214,#32215,#32216),.UNSPECIFIED.,.F.,.F.,(4,1,1,1,1,1,
1,4),(40.8407044966673,41.5878176020915,42.5666511329647,43.545484663838,
44.5243181947112,45.5031517255845,46.4819852564577,47.1238898038469),
 .UNSPECIFIED.);
#703=B_SPLINE_CURVE_WITH_KNOTS('',3,(#32221,#32222,#32223,#32224,#32225,
#32226,#32227,#32228,#32229,#32230),.UNSPECIFIED.,.F.,.F.,(4,1,1,1,1,1,
1,4),(34.5575191894877,35.1070375887762,36.0858711196495,37.0647046505227,
38.043538181396,39.0223717122692,40.0012052431424,40.8407044966673),
 .UNSPECIFIED.);
#704=B_SPLINE_CURVE_WITH_KNOTS('',3,(#32231,#32232,#32233,#32234,#32235,
#32236,#32237,#32238,#32239,#32240,#32241),.UNSPECIFIED.,.F.,.F.,(4,1,1,
1,1,1,1,1,4),(34.5575191894877,34.7359828859787,35.714816416852,36.6936499477252,
37.6724834785985,38.6513170094717,39.630150540345,40.6089840712182,40.8407044966673),
 .UNSPECIFIED.);
#705=B_SPLINE_CURVE_WITH_KNOTS('',3,(#32246,#32247,#32248,#32249,#32250,
#32251,#32252,#32253,#32254,#32255),.UNSPECIFIED.,.F.,.F.,(4,1,1,1,1,1,
1,4),(28.2743338823081,29.2340364035367,30.21286993441,31.1917034652832,
32.1705369961565,33.1493705270297,34.128204057903,34.5575191894877),
 .UNSPECIFIED.);
#706=B_SPLINE_CURVE_WITH_KNOTS('',3,(#32256,#32257,#32258,#32259,#32260,
#32261,#32262,#32263,#32264,#32265),.UNSPECIFIED.,.F.,.F.,(4,1,1,1,1,1,
1,4),(28.2743338823081,28.8629817007393,29.8418152316125,30.8206487624858,
31.799482293359,32.7783158242323,33.7571493551055,34.5575191894877),
 .UNSPECIFIED.);
#707=B_SPLINE_CURVE_WITH_KNOTS('',3,(#32270,#32271,#32272,#32273,#32274,
#32275,#32276,#32277,#32278,#32279,#32280),.UNSPECIFIED.,.F.,.F.,(4,1,1,
1,1,1,1,1,4),(21.9911485751285,22.382201687424,23.3610352182973,24.3398687491705,
25.3187022800437,26.297535810917,27.2763693417902,28.2552028726635,28.2743338823081),
 .UNSPECIFIED.);
#708=B_SPLINE_CURVE_WITH_KNOTS('',3,(#32281,#32282,#32283,#32284,#32285,
#32286,#32287,#32288,#32289,#32290,#32291),.UNSPECIFIED.,.F.,.F.,(4,1,1,
1,1,1,1,1,4),(21.9911485751285,22.0111469846265,22.9899805154998,23.968814046373,
24.9476475772463,25.9264811081195,26.9053146389928,27.884148169866,28.2743338823081),
 .UNSPECIFIED.);
#709=B_SPLINE_CURVE_WITH_KNOTS('',3,(#32296,#32297,#32298,#32299,#32300,
#32301,#32302,#32303,#32304,#32305),.UNSPECIFIED.,.F.,.F.,(4,1,1,1,1,1,
1,4),(15.7079632679489,16.5092005021845,17.4880340330578,18.466867563931,
19.4457010948043,20.4245346256775,21.4033681565508,21.9911485751285),
 .UNSPECIFIED.);
#710=B_SPLINE_CURVE_WITH_KNOTS('',3,(#32306,#32307,#32308,#32309,#32310,
#32311,#32312,#32313,#32314,#32315),.UNSPECIFIED.,.F.,.F.,(4,1,1,1,1,1,
1,4),(15.7079632679489,16.1381457993871,17.1169793302603,18.0958128611336,
19.0746463920068,20.05347992288,21.0323134537533,21.9911485751285),
 .UNSPECIFIED.);
#711=B_SPLINE_CURVE_WITH_KNOTS('',3,(#32318,#32319,#32320,#32321,#32322,
#32323,#32324,#32325,#32326,#32327,#32328,#32329,#32330,#32331,#32332,#32333,
#32334,#32335,#32336,#32337,#32338,#32339,#32340,#32341,#32342,#32343,#32344,
#32345,#32346,#32347,#32348,#32349,#32350,#32351,#32352,#32353,#32354,#32355,
#32356,#32357,#32358,#32359,#32360,#32361,#32362,#32363,#32364,#32365,#32366,
#32367,#32368,#32369,#32370,#32371,#32372,#32373,#32374,#32375,#32376,#32377,
#32378,#32379,#32380,#32381,#32382,#32383,#32384,#32385,#32386,#32387,#32388,
#32389,#32390,#32391,#32392,#32393,#32394,#32395,#32396,#32397,#32398,#32399,
#32400,#32401,#32402,#32403,#32404,#32405),.UNSPECIFIED.,.F.,.F.,(4,3,3,
3,3,3,3,3,3,3,3,3,3,3,3,3,3,3,3,3,3,3,3,3,3,3,3,3,3,4),(-0.555272788399365,
-0.52846767863439,-0.503594637637908,-0.491620530364568,-0.486548771256777,
-0.46038777702908,-0.437496907079845,-0.430089856089214,-0.425283241489225,
-0.420739109591328,-0.394172021992522,-0.367149700387639,-0.344677479649528,
-0.327654949218049,-0.322163644667068,-0.294255571126051,-0.277260817435197,
-0.250234732978329,-0.234595062167183,-0.223439460304812,-0.217840497360261,
-0.189937324364723,-0.161486698536973,-0.132774069185219,-0.116177310537067,
-0.111767824711868,-0.0823316934096331,-0.0527876353241155,-0.0237740161581124,
0.),.UNSPECIFIED.);
#712=B_SPLINE_CURVE_WITH_KNOTS('',3,(#32410,#32411,#32412,#32413,#32414,
#32415,#32416,#32417,#32418,#32419,#32420,#32421,#32422,#32423,#32424,#32425,
#32426,#32427,#32428,#32429,#32430,#32431,#32432,#32433,#32434,#32435,#32436,
#32437,#32438,#32439,#32440,#32441,#32442,#32443,#32444,#32445,#32446,#32447,
#32448,#32449,#32450,#32451,#32452,#32453,#32454,#32455,#32456,#32457,#32458,
#32459,#32460,#32461,#32462,#32463,#32464,#32465,#32466,#32467,#32468,#32469,
#32470,#32471,#32472,#32473,#32474,#32475,#32476,#32477,#32478,#32479,#32480,
#32481,#32482,#32483,#32484,#32485,#32486,#32487,#32488,#32489,#32490,#32491,
#32492,#32493,#32494,#32495,#32496,#32497,#32498,#32499,#32500,#32501,#32502,
#32503,#32504,#32505,#32506),.UNSPECIFIED.,.F.,.F.,(4,3,3,3,3,3,3,3,3,3,
3,3,3,3,3,3,3,3,3,3,3,3,3,3,3,3,3,3,3,3,3,3,4),(-0.552745378375028,-0.524051566310883,
-0.520210139258523,-0.490737208406128,-0.482065926984848,-0.476361701638012,
-0.470495789890482,-0.441459967293392,-0.417194500231044,-0.406393530772314,
-0.401030964911425,-0.39612764238736,-0.36782565203914,-0.339770953176154,
-0.316662272580769,-0.29933076213423,-0.294967834876196,-0.290936046393434,
-0.26412806323215,-0.247336230794614,-0.219938258183661,-0.192445975910703,
-0.188229859720074,-0.16160728097907,-0.135010228556239,-0.108826952648143,
-0.0998939422463041,-0.0942306910950506,-0.0901865085424749,-0.0646366135836345,
-0.0394819043305994,-0.0151075305849294,0.),.UNSPECIFIED.);
#713=B_SPLINE_CURVE_WITH_KNOTS('',3,(#32683,#32684,#32685,#32686,#32687,
#32688,#32689,#32690,#32691,#32692,#32693,#32694,#32695,#32696,#32697,#32698,
#32699,#32700,#32701),.UNSPECIFIED.,.F.,.F.,(4,3,3,3,3,3,4),(32.5332269442662,
33.2803400496904,34.2591735805636,35.2380071114369,36.2168406423101,37.1956741731834,
38.063536590894),.UNSPECIFIED.);
#714=B_SPLINE_CURVE_WITH_KNOTS('',3,(#32703,#32704,#32705,#32706,#32707,
#32708,#32709,#32710,#32711,#32712,#32713,#32714,#32715,#32716,#32717,#32718,
#32719,#32720,#32721,#32722,#32723,#32724,#32725,#32726,#32727,#32728,#32729,
#32730,#32731,#32732,#32733,#32734,#32735,#32736,#32737,#32738,#32739,#32740,
#32741,#32742,#32743,#32744,#32745,#32746,#32747,#32748,#32749,#32750,#32751,
#32752,#32753,#32754,#32755,#32756,#32757,#32758,#32759,#32760,#32761,#32762,
#32763,#32764,#32765,#32766,#32767,#32768,#32769,#32770,#32771,#32772,#32773,
#32774,#32775,#32776,#32777,#32778,#32779,#32780,#32781,#32782,#32783,#32784,
#32785,#32786,#32787,#32788,#32789,#32790),.UNSPECIFIED.,.F.,.F.,(4,3,3,
3,3,3,3,3,3,3,3,3,3,3,3,3,3,3,3,3,3,3,3,3,3,3,3,3,3,4),(-0.555272788399382,
-0.528467678634411,-0.503594611950225,-0.491620530448705,-0.486548768208902,
-0.460387774362191,-0.437496904746319,-0.430089843892791,-0.42528335746406,
-0.420739137835661,-0.394172035990758,-0.367149711920146,-0.344677488298913,
-0.327654967351694,-0.322163642962578,-0.29425557103191,-0.277260817435213,
-0.250234719828173,-0.234595049838912,-0.223439458719702,-0.217840498614478,
-0.18993731124497,-0.16148667063061,-0.132774036478808,-0.116177281918957,
-0.111767791045449,-0.0823316491114678,-0.0527875952217257,-0.0237740134204675,
0.),.UNSPECIFIED.);
#715=B_SPLINE_CURVE_WITH_KNOTS('',3,(#32791,#32792,#32793,#32794,#32795,
#32796,#32797,#32798,#32799),.UNSPECIFIED.,.F.,.F.,(4,1,1,1,1,1,4),(10.3761157273102,
11.2439781450208,12.2228116758941,13.2016452067673,14.1804787376406,15.1593122685138,
15.7079632679489),.UNSPECIFIED.);
#716=B_SPLINE_CURVE_WITH_KNOTS('',3,(#32803,#32804,#32805,#32806,#32807,
#32808,#32809,#32810),.UNSPECIFIED.,.F.,.F.,(4,1,1,1,1,4),(11.6150328478183,
12.5938663786915,13.5726999095648,14.551533440438,15.5303669713113,15.7079632679489),
 .UNSPECIFIED.);
#717=B_SPLINE_CURVE_WITH_KNOTS('',3,(#32987,#32988,#32989,#32990,#32991,
#32992,#32993,#32994,#32995,#32996,#32997,#32998,#32999,#33000,#33001,#33002,
#33003,#33004,#33005,#33006,#33007,#33008,#33009,#33010,#33011,#33012,#33013,
#33014,#33015,#33016,#33017,#33018,#33019,#33020,#33021,#33022,#33023,#33024,
#33025,#33026,#33027,#33028,#33029,#33030,#33031,#33032,#33033,#33034,#33035,
#33036,#33037,#33038,#33039,#33040,#33041,#33042,#33043,#33044,#33045,#33046,
#33047,#33048,#33049,#33050,#33051,#33052,#33053,#33054,#33055,#33056,#33057,
#33058,#33059,#33060,#33061,#33062,#33063,#33064,#33065,#33066,#33067,#33068,
#33069,#33070,#33071,#33072,#33073,#33074,#33075,#33076,#33077,#33078,#33079,
#33080,#33081,#33082,#33083),.UNSPECIFIED.,.F.,.F.,(4,3,3,3,3,3,3,3,3,3,
3,3,3,3,3,3,3,3,3,3,3,3,3,3,3,3,3,3,3,3,3,3,4),(-0.552745378375046,-0.524051576025582,
-0.520210139258547,-0.490737207720614,-0.482065932922306,-0.476361784855821,
-0.470495811804092,-0.441459989540148,-0.417194519696956,-0.406393563117289,
-0.401031128507146,-0.396127678339415,-0.367825690719443,-0.339771006600577,
-0.316662312649086,-0.299330792185467,-0.294967891446945,-0.290936172565379,
-0.264128215008968,-0.247336230794613,-0.219938271840149,-0.192445987860131,
-0.188229859754739,-0.161607289273899,-0.135010221728073,-0.108826909841477,
-0.0998938267520413,-0.0942311920104265,-0.0901865995336686,-0.0646366752402619,
-0.0394819229126391,-0.0151074961268136,0.),.UNSPECIFIED.);
#718=B_SPLINE_CURVE_WITH_KNOTS('',3,(#33084,#33085,#33086,#33087,#33088,
#33089,#33090,#33091,#33092,#33093,#33094,#33095,#33096,#33097,#33098,#33099),
 .UNSPECIFIED.,.F.,.F.,(4,3,3,3,3,4),(-40.1321747658031,-39.1533412349299,
-38.1745077040566,-37.1956741731834,-36.2168406423101,-35.5088569560286),
 .UNSPECIFIED.);
#719=B_SPLINE_CURVE_WITH_KNOTS('',3,(#33230,#33231,#33232,#33233,#33234,
#33235,#33236,#33237,#33238,#33239,#33240,#33241,#33242,#33243,#33244,#33245,
#33246,#33247,#33248),.UNSPECIFIED.,.F.,.F.,(4,3,3,3,3,3,4),(-0.113329393083273,
-0.0991044193051623,-0.0674458844185764,-0.061631000326846,-0.0331038403136512,
-0.00584534044920819,0.),.UNSPECIFIED.);
#720=B_SPLINE_CURVE_WITH_KNOTS('',3,(#33252,#33253,#33254,#33255,#33256,
#33257,#33258,#33259,#33260,#33261,#33262,#33263,#33264,#33265,#33266,#33267,
#33268,#33269,#33270,#33271,#33272,#33273,#33274,#33275,#33276,#33277,#33278,
#33279,#33280,#33281,#33282),.UNSPECIFIED.,.F.,.F.,(4,3,3,3,3,3,3,3,3,3,
4),(-0.226650511587635,-0.198574388081722,-0.170498264575808,-0.13944012666617,
-0.131476509591221,-0.0991044193051576,-0.0762723334429418,-0.0616310003268515,
-0.0331662800001561,-0.00604790654757715,0.),.UNSPECIFIED.);
#721=B_SPLINE_CURVE_WITH_KNOTS('',3,(#33286,#33287,#33288,#33289,#33290,
#33291,#33292,#33293,#33294,#33295,#33296,#33297,#33298,#33299,#33300,#33301,
#33302,#33303,#33304,#33305,#33306,#33307,#33308,#33309,#33310,#33311,#33312,
#33313,#33314,#33315,#33316),.UNSPECIFIED.,.F.,.F.,(4,3,3,3,3,3,3,3,3,3,
4),(-0.226650511587582,-0.198574388081676,-0.170498264575771,-0.13944012666705,
-0.131476509591215,-0.0991044193051536,-0.0762723334429342,-0.0616310003268419,
-0.0331662799998172,-0.00604790654743552,0.),.UNSPECIFIED.);
#722=B_SPLINE_CURVE_WITH_KNOTS('',3,(#33320,#33321,#33322,#33323,#33324,
#33325,#33326,#33327,#33328,#33329,#33330,#33331,#33332,#33333,#33334,#33335,
#33336,#33337,#33338,#33339,#33340,#33341,#33342,#33343,#33344,#33345,#33346,
#33347,#33348,#33349,#33350),.UNSPECIFIED.,.F.,.F.,(4,3,3,3,3,3,3,3,3,3,
4),(-0.226650511587584,-0.198574388081659,-0.170498264575734,-0.139440596738821,
-0.131476509591163,-0.0991044193051282,-0.0762723334429448,-0.0616310003268502,
-0.0331645723826234,-0.00604411953936661,0.),.UNSPECIFIED.);
#723=B_SPLINE_CURVE_WITH_KNOTS('',3,(#33354,#33355,#33356,#33357,#33358,
#33359,#33360,#33361,#33362,#33363,#33364,#33365,#33366,#33367,#33368,#33369,
#33370,#33371,#33372,#33373,#33374,#33375,#33376,#33377,#33378,#33379,#33380,
#33381,#33382,#33383,#33384),.UNSPECIFIED.,.F.,.F.,(4,3,3,3,3,3,3,3,3,3,
4),(-0.226650511587706,-0.198574388081775,-0.170498264575844,-0.139440126665696,
-0.131476509591268,-0.0991044193051773,-0.0762723334429522,-0.0616310003268415,
-0.0331662800006236,-0.00604790654845245,0.),.UNSPECIFIED.);
#724=B_SPLINE_CURVE_WITH_KNOTS('',3,(#33388,#33389,#33390,#33391,#33392,
#33393,#33394,#33395,#33396,#33397,#33398,#33399,#33400,#33401,#33402,#33403,
#33404,#33405,#33406,#33407,#33408,#33409,#33410,#33411,#33412,#33413,#33414,
#33415,#33416,#33417,#33418),.UNSPECIFIED.,.F.,.F.,(4,3,3,3,3,3,3,3,3,3,
4),(-0.226650511587727,-0.198574388081779,-0.170498264575831,-0.139440126665785,
-0.13147650959124,-0.0991044193051654,-0.0762723334429508,-0.0616310003268513,
-0.0331662799998889,-0.00604790654758933,0.),.UNSPECIFIED.);
#725=B_SPLINE_CURVE_WITH_KNOTS('',3,(#33421,#33422,#33423,#33424,#33425,
#33426,#33427,#33428,#33429,#33430,#33431,#33432,#33433,#33434,#33435,#33436),
 .UNSPECIFIED.,.F.,.F.,(4,3,3,3,3,4),(-0.226650511587688,-0.198574388081761,
-0.170498264575834,-0.150386414929284,-0.131476509591241,-0.113329393083273),
 .UNSPECIFIED.);
#726=B_SPLINE_CURVE_WITH_KNOTS('',3,(#33458,#33459,#33460,#33461),
 .UNSPECIFIED.,.F.,.F.,(4,4),(0.474834937773607,0.639817807990862),
 .UNSPECIFIED.);
#727=B_SPLINE_CURVE_WITH_KNOTS('',3,(#33463,#33464,#33465,#33466,#33467,
#33468),.UNSPECIFIED.,.F.,.F.,(4,2,4),(-0.0356915196979304,-0.0178436364936306,
0.),.UNSPECIFIED.);
#728=B_SPLINE_CURVE_WITH_KNOTS('',3,(#33470,#33471,#33472,#33473,#33474),
 .UNSPECIFIED.,.F.,.F.,(4,1,4),(-0.63803777562903,-0.309114526274187,-0.0628670973485611),
 .UNSPECIFIED.);
#729=B_SPLINE_CURVE_WITH_KNOTS('',3,(#33476,#33477,#33478,#33479,#33480,
#33481),.UNSPECIFIED.,.F.,.F.,(4,2,4),(-0.035691517766977,-0.0178476663798058,
0.),.UNSPECIFIED.);
#730=B_SPLINE_CURVE_WITH_KNOTS('',3,(#33482,#33483,#33484,#33485),
 .UNSPECIFIED.,.F.,.F.,(4,4),(0.0610870649866808,0.226069935203935),
 .UNSPECIFIED.);
#731=B_SPLINE_CURVE_WITH_KNOTS('',3,(#33507,#33508,#33509,#33510),
 .UNSPECIFIED.,.F.,.F.,(4,4),(0.474834937773608,0.639817807990862),
 .UNSPECIFIED.);
#732=B_SPLINE_CURVE_WITH_KNOTS('',3,(#33512,#33513,#33514,#33515,#33516,
#33517),.UNSPECIFIED.,.F.,.F.,(4,2,4),(-0.0356915197043745,-0.0178436364953559,
0.),.UNSPECIFIED.);
#733=B_SPLINE_CURVE_WITH_KNOTS('',3,(#33519,#33520,#33521,#33522,#33523),
 .UNSPECIFIED.,.F.,.F.,(4,1,4),(-0.638037775629031,-0.309114526274187,-0.062867097348561),
 .UNSPECIFIED.);
#734=B_SPLINE_CURVE_WITH_KNOTS('',3,(#33524,#33525,#33526,#33527,#33528,
#33529),.UNSPECIFIED.,.F.,.F.,(4,2,4),(-0.0356915177684809,-0.0178476663801996,
0.),.UNSPECIFIED.);
#735=B_SPLINE_CURVE_WITH_KNOTS('',3,(#33530,#33531,#33532,#33533),
 .UNSPECIFIED.,.F.,.F.,(4,4),(0.0610870649866807,0.226069935203935),
 .UNSPECIFIED.);
#736=B_SPLINE_CURVE_WITH_KNOTS('',3,(#33536,#33537,#33538,#33539),
 .UNSPECIFIED.,.F.,.F.,(4,4),(0.061087064986681,0.226069935203935),
 .UNSPECIFIED.);
#737=B_SPLINE_CURVE_WITH_KNOTS('',3,(#33542,#33543,#33544,#33545),
 .UNSPECIFIED.,.F.,.F.,(4,4),(0.0610870649866804,0.226069935203935),
 .UNSPECIFIED.);
#738=B_SPLINE_CURVE_WITH_KNOTS('',3,(#33546,#33547,#33548,#33549),
 .UNSPECIFIED.,.F.,.F.,(4,4),(0.474834937773607,0.639817807990862),
 .UNSPECIFIED.);
#739=B_SPLINE_CURVE_WITH_KNOTS('',3,(#33552,#33553,#33554,#33555),
 .UNSPECIFIED.,.F.,.F.,(4,4),(0.0610870649866807,0.226069935203935),
 .UNSPECIFIED.);
#740=B_SPLINE_CURVE_WITH_KNOTS('',3,(#33556,#33557,#33558,#33559),
 .UNSPECIFIED.,.F.,.F.,(4,4),(0.474834937773607,0.639817807990861),
 .UNSPECIFIED.);
#741=B_SPLINE_CURVE_WITH_KNOTS('',3,(#33562,#33563,#33564,#33565),
 .UNSPECIFIED.,.F.,.F.,(4,4),(0.0610870649866801,0.226069935203935),
 .UNSPECIFIED.);
#742=B_SPLINE_CURVE_WITH_KNOTS('',3,(#33566,#33567,#33568,#33569),
 .UNSPECIFIED.,.F.,.F.,(4,4),(0.474834937773608,0.639817807990862),
 .UNSPECIFIED.);
#743=B_SPLINE_CURVE_WITH_KNOTS('',3,(#33571,#33572,#33573,#33574),
 .UNSPECIFIED.,.F.,.F.,(4,4),(0.474834937773608,0.639817807990862),
 .UNSPECIFIED.);
#744=B_SPLINE_CURVE_WITH_KNOTS('',3,(#33596,#33597,#33598,#33599,#33600,
#33601),.UNSPECIFIED.,.F.,.F.,(4,2,4),(-0.0356915197030877,-0.0178436364955222,
0.),.UNSPECIFIED.);
#745=B_SPLINE_CURVE_WITH_KNOTS('',3,(#33603,#33604,#33605,#33606,#33607),
 .UNSPECIFIED.,.F.,.F.,(4,1,4),(-0.63803777562903,-0.309114526274187,-0.0628670973485611),
 .UNSPECIFIED.);
#746=B_SPLINE_CURVE_WITH_KNOTS('',3,(#33608,#33609,#33610,#33611,#33612,
#33613),.UNSPECIFIED.,.F.,.F.,(4,2,4),(-0.0356915177637329,-0.0178476663792099,
0.),.UNSPECIFIED.);
#747=B_SPLINE_CURVE_WITH_KNOTS('',3,(#33618,#33619,#33620,#33621,#33622,
#33623),.UNSPECIFIED.,.F.,.F.,(4,2,4),(-0.0356915177685627,-0.0178476663800234,
0.),.UNSPECIFIED.);
#748=B_SPLINE_CURVE_WITH_KNOTS('',3,(#33629,#33630,#33631,#33632,#33633,
#33634),.UNSPECIFIED.,.F.,.F.,(4,2,4),(-0.035691519698345,-0.0178436364936918,
0.),.UNSPECIFIED.);
#749=B_SPLINE_CURVE_WITH_KNOTS('',3,(#33636,#33637,#33638,#33639,#33640,
#33641),.UNSPECIFIED.,.F.,.F.,(4,2,4),(-0.0356915177661021,-0.0178476663801455,
0.),.UNSPECIFIED.);
#750=B_SPLINE_CURVE_WITH_KNOTS('',3,(#33646,#33647,#33648,#33649,#33650,
#33651),.UNSPECIFIED.,.F.,.F.,(4,2,4),(-0.0356915197010578,-0.0178436364947975,
0.),.UNSPECIFIED.);
#751=B_SPLINE_CURVE_WITH_KNOTS('',3,(#33654,#33655,#33656,#33657,#33658,
#33659),.UNSPECIFIED.,.F.,.F.,(4,2,4),(-0.0356915196998398,-0.0178436364940569,
0.),.UNSPECIFIED.);
#752=B_SPLINE_CURVE_WITH_KNOTS('',3,(#33661,#33662,#33663,#33664,#33665,
#33666),.UNSPECIFIED.,.F.,.F.,(4,2,4),(-0.0356915177634285,-0.0178476663777042,
0.),.UNSPECIFIED.);
#753=B_SPLINE_CURVE_WITH_KNOTS('',3,(#33688,#33689,#33690,#33691,#33692),
 .UNSPECIFIED.,.F.,.F.,(4,1,4),(-0.63803777562903,-0.309114526274187,-0.0628670973485611),
 .UNSPECIFIED.);
#754=B_SPLINE_CURVE_WITH_KNOTS('',3,(#33721,#33722,#33723,#33724,#33725),
 .UNSPECIFIED.,.F.,.F.,(4,1,4),(-0.638037775629031,-0.391790346703356,-0.0628670973485609),
 .UNSPECIFIED.);
#755=B_SPLINE_CURVE_WITH_KNOTS('',3,(#33762,#33763,#33764,#33765,#33766),
 .UNSPECIFIED.,.F.,.F.,(4,1,4),(-0.63803777562903,-0.309114526274187,-0.0628670973485611),
 .UNSPECIFIED.);
#756=B_SPLINE_CURVE_WITH_KNOTS('',3,(#34523,#34524,#34525,#34526,#34527,
#34528,#34529,#34530,#34531,#34532,#34533,#34534,#34535,#34536,#34537,#34538,
#34539,#34540,#34541,#34542,#34543,#34544,#34545,#34546,#34547,#34548,#34549,
#34550,#34551,#34552,#34553,#34554,#34555,#34556,#34557,#34558,#34559,#34560,
#34561,#34562,#34563,#34564,#34565,#34566,#34567,#34568,#34569,#34570,#34571,
#34572,#34573,#34574,#34575,#34576,#34577,#34578,#34579,#34580,#34581,#34582,
#34583,#34584,#34585),.UNSPECIFIED.,.F.,.F.,(4,1,1,1,1,1,1,1,1,1,1,1,1,
1,1,1,1,1,1,1,1,1,1,1,1,1,1,1,1,1,1,1,1,1,1,1,1,1,1,1,1,1,1,1,1,1,1,1,1,
1,1,1,1,1,1,1,1,1,1,1,4),(0.,0.00892857142857143,0.0178571428571429,0.0357142857142857,
0.0535714285714286,0.0714285714285714,0.0892857142857143,0.107142857142857,
0.125,0.142857142857143,0.154761904761905,0.166666666666667,0.178571428571429,
0.19047619047619,0.202380952380952,0.214285714285714,0.238095238095238,
0.261904761904762,0.273809523809524,0.285714285714286,0.30952380952381,
0.333333333333333,0.357142857142857,0.369047619047619,0.380952380952381,
0.392857142857143,0.404761904761905,0.416666666666667,0.428571428571429,
0.446428571428571,0.464285714285714,0.482142857142857,0.5,0.517857142857143,
0.535714285714286,0.553571428571429,0.571428571428571,0.589285714285714,
0.607142857142857,0.625,0.642857142857143,0.660714285714286,0.678571428571428,
0.696428571428571,0.714285714285714,0.726190476190476,0.738095238095238,
0.761904761904762,0.785714285714286,0.809523809523809,0.833333333333333,
0.857142857142857,0.875,0.892857142857143,0.910714285714286,0.928571428571429,
0.946428571428571,0.964285714285714,0.982142857142857,0.991071428571429,
1.),.UNSPECIFIED.);
#757=B_SPLINE_CURVE_WITH_KNOTS('',3,(#34595,#34596,#34597,#34598,#34599,
#34600,#34601,#34602,#34603,#34604),.UNSPECIFIED.,.F.,.F.,(4,3,3,4),(-4.09157007060746,
-3.99669758015803,-2.99752318511852,-2.06659765062436),.UNSPECIFIED.);
#758=B_SPLINE_CURVE_WITH_KNOTS('',3,(#34607,#34608,#34609,#34610,#34611,
#34612,#34613),.UNSPECIFIED.,.F.,.F.,(4,3,4),(0.,0.999174395039508,1.11662023360669),
 .UNSPECIFIED.);
#759=B_SPLINE_CURVE_WITH_KNOTS('',3,(#34618,#34619,#34620,#34621,#34622,
#34623,#34624,#34625,#34626,#34627,#34628,#34629,#34630,#34631,#34632,#34633,
#34634,#34635,#34636,#34637,#34638,#34639),.UNSPECIFIED.,.F.,.F.,(4,3,3,
3,3,3,3,4),(-10.3747553777871,-9.99174395039507,-8.99256955535556,-7.99339516031606,
-6.99422076527655,-5.99504637023704,-4.99587197519754,-4.09157007060746),
 .UNSPECIFIED.);
#760=B_SPLINE_CURVE_WITH_KNOTS('',3,(#34640,#34641,#34642,#34643,#34644,
#34645,#34646,#34647,#34648,#34649,#34650,#34651,#34652,#34653,#34654,#34655,
#34656,#34657,#34658,#34659,#34660,#34661),.UNSPECIFIED.,.F.,.F.,(4,3,3,
3,3,3,3,4),(1.11662023360669,1.99834879007901,2.99752318511852,3.99669758015803,
4.99587197519753,5.99504637023704,6.99422076527654,7.39980554078627),
 .UNSPECIFIED.);
#761=B_SPLINE_CURVE_WITH_KNOTS('',3,(#34666,#34667,#34668,#34669,#34670,
#34671,#34672,#34673,#34674,#34675,#34676,#34677,#34678,#34679,#34680,#34681,
#34682,#34683,#34684,#34685,#34686,#34687),.UNSPECIFIED.,.F.,.F.,(4,3,3,
3,3,3,3,4),(-16.6579406849666,-15.9867903206321,-14.9876159255926,-13.9884415305531,
-12.9892671355136,-11.9900927404741,-10.9909183454346,-10.3747553777871),
 .UNSPECIFIED.);
#762=B_SPLINE_CURVE_WITH_KNOTS('',3,(#34688,#34689,#34690,#34691,#34692,
#34693,#34694,#34695,#34696,#34697,#34698,#34699,#34700,#34701,#34702,#34703,
#34704,#34705,#34706,#34707,#34708,#34709),.UNSPECIFIED.,.F.,.F.,(4,3,3,
3,3,3,3,4),(7.39980554078627,7.99339516031605,8.99256955535556,9.99174395039507,
10.9909183454346,11.9900927404741,12.9892671355136,13.6829908479659),
 .UNSPECIFIED.);
#763=B_SPLINE_CURVE_WITH_KNOTS('',3,(#34714,#34715,#34716,#34717,#34718,
#34719,#34720,#34721,#34722,#34723,#34724,#34725,#34726,#34727,#34728,#34729,
#34730,#34731,#34732,#34733,#34734,#34735),.UNSPECIFIED.,.F.,.F.,(4,3,3,
3,3,3,3,4),(-22.9411259921462,-21.9818366908691,-20.9826622958296,-19.9834879007901,
-18.9843135057506,-17.9851391107111,-16.9859647156716,-16.6579406849666),
 .UNSPECIFIED.);
#764=B_SPLINE_CURVE_WITH_KNOTS('',3,(#34736,#34737,#34738,#34739,#34740,
#34741,#34742,#34743,#34744,#34745,#34746,#34747,#34748,#34749,#34750,#34751,
#34752,#34753,#34754,#34755,#34756,#34757),.UNSPECIFIED.,.F.,.F.,(4,3,3,
3,3,3,3,4),(13.6829908479659,13.9884415305531,14.9876159255926,15.9867903206321,
16.9859647156716,17.9851391107111,18.9843135057506,19.9661761551454),
 .UNSPECIFIED.);
#765=B_SPLINE_CURVE_WITH_KNOTS('',3,(#34763,#34764,#34765,#34766,#34767,
#34768,#34769),.UNSPECIFIED.,.F.,.F.,(4,1,1,1,4),(34.5575191894877,34.5974042832501,
35.5965786782897,36.5957530733292,37.5266786078233),.UNSPECIFIED.);
#766=B_SPLINE_CURVE_WITH_KNOTS('',3,(#34772,#34773,#34774,#34775,#34776),
 .UNSPECIFIED.,.F.,.F.,(4,1,4),(34.5575191894877,35.2858663932294,36.2850407882689),
 .UNSPECIFIED.);
#767=B_SPLINE_CURVE_WITH_KNOTS('',3,(#34781,#34782,#34783,#34784,#34785,
#34786,#34787,#34788,#34789,#34790),.UNSPECIFIED.,.F.,.F.,(4,1,1,1,1,1,
1,4),(28.2743338823081,28.6023579130131,29.6015323080526,30.6007067030921,
31.5998810981316,32.5990554931711,33.5982298882106,34.5575191894877),
 .UNSPECIFIED.);
#768=B_SPLINE_CURVE_WITH_KNOTS('',3,(#34791,#34792,#34793,#34794,#34795,
#34796,#34797,#34798,#34799,#34800,#34801),.UNSPECIFIED.,.F.,.F.,(4,1,1,
1,1,1,1,1,4),(28.2743338823081,28.2916456279528,29.2908200229923,30.2899944180318,
31.2891688130713,32.2883432081108,33.2875176031503,34.2866919981899,34.5575191894877),
 .UNSPECIFIED.);
#769=B_SPLINE_CURVE_WITH_KNOTS('',3,(#34806,#34807,#34808,#34809,#34810,
#34811,#34812,#34813,#34814,#34815),.UNSPECIFIED.,.F.,.F.,(4,1,1,1,1,1,
1,4),(21.9911485751285,22.6073115427761,23.6064859378156,24.6056603328551,
25.6048347278946,26.6040091229341,27.6031835179736,28.2743338823081),
 .UNSPECIFIED.);
#770=B_SPLINE_CURVE_WITH_KNOTS('',3,(#34816,#34817,#34818,#34819,#34820,
#34821,#34822,#34823,#34824,#34825),.UNSPECIFIED.,.F.,.F.,(4,1,1,1,1,1,
1,4),(21.9911485751285,22.2965992577158,23.2957736527553,24.2949480477948,
25.2941224428343,26.2932968378738,27.2924712329133,28.2743338823081),
 .UNSPECIFIED.);
#771=B_SPLINE_CURVE_WITH_KNOTS('',3,(#34830,#34831,#34832,#34833,#34834,
#34835,#34836,#34837,#34838,#34839),.UNSPECIFIED.,.F.,.F.,(4,1,1,1,1,1,
1,4),(15.707963267949,16.612265172539,17.6114395675785,18.610613962618,
19.6097883576575,20.6089627526971,21.6081371477366,21.9911485751285),
 .UNSPECIFIED.);
#772=B_SPLINE_CURVE_WITH_KNOTS('',3,(#34840,#34841,#34842,#34843,#34844,
#34845,#34846,#34847,#34848,#34849),.UNSPECIFIED.,.F.,.F.,(4,1,1,1,1,1,
1,4),(15.707963267949,16.3015528874787,17.3007272825182,18.2999016775577,
19.2990760725973,20.2982504676368,21.2974248626763,21.9911485751285),
 .UNSPECIFIED.);
#773=B_SPLINE_CURVE_WITH_KNOTS('',3,(#34852,#34853,#34854,#34855,#34856,
#34857,#34858,#34859,#34860,#34861,#34862,#34863,#34864,#34865,#34866,#34867,
#34868,#34869,#34870,#34871,#34872,#34873,#34874,#34875,#34876,#34877,#34878,
#34879,#34880,#34881,#34882,#34883,#34884,#34885,#34886,#34887,#34888,#34889,
#34890,#34891,#34892,#34893,#34894,#34895,#34896,#34897,#34898,#34899,#34900,
#34901,#34902,#34903,#34904,#34905,#34906,#34907,#34908,#34909,#34910,#34911,
#34912,#34913,#34914,#34915,#34916,#34917,#34918,#34919,#34920,#34921,#34922,
#34923,#34924,#34925,#34926,#34927,#34928,#34929,#34930,#34931,#34932,#34933,
#34934,#34935,#34936,#34937,#34938,#34939),.UNSPECIFIED.,.F.,.F.,(4,3,3,
3,3,3,3,3,3,3,3,3,3,3,3,3,3,3,3,3,3,3,3,3,3,3,3,3,3,4),(-0.463803050843695,
-0.449990761124198,-0.428296524385296,-0.416270113415759,-0.41034182721078,
-0.406031993683804,-0.383353142504459,-0.364918243300489,-0.357623436893478,
-0.352445440792161,-0.329117850494041,-0.305348418252453,-0.287979800907514,
-0.27495333789881,-0.271003592095896,-0.246574718000476,-0.235873948872699,
-0.212294861299806,-0.188221669997877,-0.184247659311273,-0.180472049728776,
-0.156013909098849,-0.131078945975368,-0.105968578777427,-0.0960005902951454,
-0.0910052533817002,-0.0652636023140419,-0.03948256399711,-0.0142485222596106,
0.),.UNSPECIFIED.);
#774=B_SPLINE_CURVE_WITH_KNOTS('',3,(#34944,#34945,#34946,#34947,#34948,
#34949,#34950,#34951,#34952,#34953,#34954,#34955,#34956,#34957,#34958,#34959,
#34960,#34961,#34962,#34963,#34964,#34965,#34966,#34967,#34968,#34969,#34970,
#34971,#34972,#34973,#34974,#34975,#34976,#34977,#34978,#34979,#34980,#34981,
#34982,#34983,#34984,#34985,#34986,#34987,#34988,#34989,#34990,#34991,#34992,
#34993,#34994,#34995,#34996,#34997,#34998,#34999,#35000,#35001,#35002,#35003,
#35004,#35005,#35006,#35007,#35008,#35009,#35010,#35011,#35012,#35013,#35014,
#35015,#35016,#35017,#35018,#35019,#35020,#35021,#35022,#35023,#35024,#35025,
#35026,#35027,#35028,#35029,#35030,#35031),.UNSPECIFIED.,.F.,.F.,(4,3,3,
3,3,3,3,3,3,3,3,3,3,3,3,3,3,3,3,3,3,3,3,3,3,3,3,3,3,4),(-0.46178896489977,
-0.445096409523187,-0.41948010739612,-0.406506945826406,-0.398412550454382,
-0.393270804127913,-0.367882741380425,-0.348386088992959,-0.338710078205615,
-0.332907547801024,-0.308142244019199,-0.283899773513071,-0.26018963968495,
-0.251870459427571,-0.247081329031836,-0.243331119007966,-0.219855106139638,
-0.211909522280695,-0.187951737144655,-0.164457770001573,-0.15868347025795,
-0.135324913286723,-0.111987831540051,-0.0890431146252489,-0.0803312568299254,
-0.0766174929132729,-0.0541552161857382,-0.0320577725876878,-0.0106683587118627,
0.),.UNSPECIFIED.);
#775=B_SPLINE_CURVE_WITH_KNOTS('',3,(#35156,#35157,#35158,#35159,#35160,
#35161,#35162,#35163,#35164,#35165,#35166,#35167,#35168,#35169,#35170,#35171,
#35172,#35173,#35174,#35175,#35176,#35177),.UNSPECIFIED.,.F.,.F.,(4,3,3,
3,3,3,3,4),(19.9661761551454,19.9834879007901,20.9826622958296,21.9818366908691,
22.9810110859087,23.9801854809482,24.9793598759877,25.9102854104818),
 .UNSPECIFIED.);
#776=B_SPLINE_CURVE_WITH_KNOTS('',3,(#35179,#35180,#35181,#35182,#35183,
#35184,#35185,#35186,#35187,#35188,#35189,#35190,#35191,#35192,#35193,#35194,
#35195,#35196,#35197,#35198,#35199,#35200,#35201,#35202,#35203,#35204,#35205,
#35206,#35207,#35208,#35209,#35210,#35211,#35212,#35213,#35214,#35215,#35216,
#35217,#35218,#35219,#35220,#35221,#35222,#35223,#35224,#35225,#35226,#35227,
#35228,#35229,#35230,#35231,#35232,#35233,#35234,#35235,#35236,#35237,#35238,
#35239,#35240,#35241,#35242,#35243,#35244,#35245,#35246,#35247,#35248,#35249,
#35250,#35251,#35252,#35253,#35254,#35255,#35256,#35257,#35258,#35259,#35260,
#35261,#35262,#35263,#35264,#35265,#35266),.UNSPECIFIED.,.F.,.F.,(4,3,3,
3,3,3,3,3,3,3,3,3,3,3,3,3,3,3,3,3,3,3,3,3,3,3,3,3,3,4),(-0.463803050843709,
-0.449990761124214,-0.428296490111524,-0.416270081284097,-0.410341690806036,
-0.406031962003142,-0.383353089621238,-0.364918197027671,-0.357623306842884,
-0.35244540774759,-0.329117799946646,-0.305348369315656,-0.287979764204916,
-0.274953310371862,-0.271003565635767,-0.246574693089584,-0.235873948872699,
-0.21229484773092,-0.188221640039157,-0.184247642913191,-0.180472048117772,
-0.15601389132531,-0.131078912920519,-0.105968544178087,-0.096000611432122,
-0.0910052576643347,-0.0652635971708748,-0.0394825672375708,-0.014248568646013,
0.),.UNSPECIFIED.);
#777=B_SPLINE_CURVE_WITH_KNOTS('',3,(#35267,#35268,#35269,#35270,#35271,
#35272,#35273,#35274,#35275),.UNSPECIFIED.,.F.,.F.,(4,1,1,1,1,1,4),(10.374755377787,
11.3056809122812,12.3048553073207,13.3040297023602,14.3032040973997,15.3023784924392,
15.707963267949),.UNSPECIFIED.);
#778=B_SPLINE_CURVE_WITH_KNOTS('',3,(#35281,#35282,#35283,#35284,#35285,
#35286,#35287,#35288,#35289,#35290,#35291,#35292,#35293,#35294,#35295,#35296,
#35297,#35298,#35299,#35300,#35301,#35302,#35303,#35304,#35305,#35306,#35307,
#35308,#35309,#35310,#35311,#35312,#35313,#35314,#35315,#35316,#35317,#35318,
#35319,#35320,#35321,#35322,#35323,#35324,#35325,#35326,#35327,#35328,#35329,
#35330,#35331,#35332,#35333,#35334,#35335,#35336,#35337,#35338,#35339,#35340,
#35341,#35342,#35343,#35344,#35345,#35346,#35347,#35348,#35349,#35350,#35351,
#35352,#35353,#35354,#35355,#35356,#35357,#35358,#35359,#35360,#35361,#35362,
#35363,#35364,#35365,#35366,#35367,#35368),.UNSPECIFIED.,.F.,.F.,(4,3,3,
3,3,3,3,3,3,3,3,3,3,3,3,3,3,3,3,3,3,3,3,3,3,3,3,3,3,4),(-0.461788964899768,
-0.445096409523188,-0.419480109352795,-0.406506947660789,-0.398412571668129,
-0.393270813953603,-0.367882751783358,-0.348386098095525,-0.338710098423989,
-0.332907549361998,-0.308142248257406,-0.283899804164729,-0.260189710156508,
-0.251870630384198,-0.247081550599562,-0.243331158606442,-0.219855173637982,
-0.211909522280694,-0.187951756384898,-0.164457786836786,-0.158683460701996,
-0.135324913663822,-0.111987815902327,-0.0890430596778552,-0.0803312466615788,
-0.0766174883386559,-0.0541551823514923,-0.0320576942341872,-0.0106682241746107,
0.),.UNSPECIFIED.);
#779=B_SPLINE_CURVE_WITH_KNOTS('',3,(#35371,#35372,#35373,#35374,#35375,
#35376,#35377,#35378),.UNSPECIFIED.,.F.,.F.,(4,1,1,1,1,4),(11.6163931973415,
12.615567592381,13.6147419874205,14.61391638246,15.6130907774995,15.707963267949),
 .UNSPECIFIED.);
#780=B_SPLINE_CURVE_WITH_KNOTS('',3,(#35503,#35504,#35505,#35506,#35507,
#35508,#35509,#35510,#35511,#35512,#35513,#35514,#35515,#35516,#35517,#35518,
#35519,#35520,#35521),.UNSPECIFIED.,.F.,.F.,(4,3,3,3,3,3,4),(-27.9768830611062,
-26.9777086660667,-25.9785342710272,-24.9793598759877,-23.9801854809482,
-22.9810110859087,-22.9411259921462),.UNSPECIFIED.);
#781=B_SPLINE_CURVE_WITH_KNOTS('',3,(#35577,#35578,#35579,#35580,#35581,
#35582,#35583,#35584,#35585,#35586),.UNSPECIFIED.,.F.,.F.,(4,3,3,4),(-4.09157007060748,
-3.98134283811107,-2.9860071285833,-2.06659765062437),.UNSPECIFIED.);
#782=B_SPLINE_CURVE_WITH_KNOTS('',3,(#35589,#35590,#35591,#35592,#35593,
#35594,#35595),.UNSPECIFIED.,.F.,.F.,(4,3,4),(0.,0.995335709527768,1.1166202336066),
 .UNSPECIFIED.);
#783=B_SPLINE_CURVE_WITH_KNOTS('',3,(#35600,#35601,#35602,#35603,#35604,
#35605,#35606,#35607,#35608,#35609,#35610,#35611,#35612,#35613,#35614,#35615,
#35616,#35617,#35618,#35619,#35620,#35621),.UNSPECIFIED.,.F.,.F.,(4,3,3,
3,3,3,3,4),(-10.3747553777871,-9.95335709527767,-8.9580213857499,-7.96268567622213,
-6.96734996669437,-5.9720142571666,-4.97667854763883,-4.09157007060748),
 .UNSPECIFIED.);
#784=B_SPLINE_CURVE_WITH_KNOTS('',3,(#35622,#35623,#35624,#35625,#35626,
#35627,#35628,#35629,#35630,#35631,#35632,#35633,#35634,#35635,#35636,#35637,
#35638,#35639,#35640,#35641,#35642,#35643),.UNSPECIFIED.,.F.,.F.,(4,3,3,
3,3,3,3,4),(1.1166202336066,1.99067141905553,2.9860071285833,3.98134283811107,
4.97667854763883,5.9720142571666,6.96734996669436,7.39980554078619),
 .UNSPECIFIED.);
#785=B_SPLINE_CURVE_WITH_KNOTS('',3,(#35648,#35649,#35650,#35651,#35652,
#35653,#35654,#35655,#35656,#35657,#35658,#35659,#35660,#35661,#35662,#35663,
#35664,#35665,#35666,#35667,#35668,#35669),.UNSPECIFIED.,.F.,.F.,(4,3,3,
3,3,3,3,4),(-16.6579406849666,-15.9253713524443,-14.9300356429165,-13.9346999333887,
-12.939364223861,-11.9440285143332,-10.9486928048054,-10.3747553777871),
 .UNSPECIFIED.);
#786=B_SPLINE_CURVE_WITH_KNOTS('',3,(#35670,#35671,#35672,#35673,#35674,
#35675,#35676,#35677,#35678,#35679,#35680,#35681,#35682,#35683,#35684,#35685,
#35686,#35687,#35688,#35689,#35690,#35691),.UNSPECIFIED.,.F.,.F.,(4,3,3,
3,3,3,3,4),(7.39980554078619,7.96268567622213,8.9580213857499,9.95335709527766,
10.9486928048054,11.9440285143332,12.939364223861,13.6829908479658),
 .UNSPECIFIED.);
#787=B_SPLINE_CURVE_WITH_KNOTS('',3,(#35696,#35697,#35698,#35699,#35700,
#35701,#35702,#35703,#35704,#35705,#35706,#35707,#35708,#35709,#35710,#35711,
#35712,#35713,#35714,#35715,#35716,#35717,#35718,#35719,#35720),
 .UNSPECIFIED.,.F.,.F.,(4,3,3,3,3,3,3,3,4),(-22.9411259921462,-22.8927213191386,
-21.8973856096109,-20.9020499000831,-19.9067141905553,-18.9113784810276,
-17.9160427714998,-16.920707061972,-16.6579406849666),.UNSPECIFIED.);
#788=B_SPLINE_CURVE_WITH_KNOTS('',3,(#35721,#35722,#35723,#35724,#35725,
#35726,#35727,#35728,#35729,#35730,#35731,#35732,#35733,#35734,#35735,#35736,
#35737,#35738,#35739,#35740,#35741,#35742,#35743,#35744,#35745),
 .UNSPECIFIED.,.F.,.F.,(4,3,3,3,3,3,3,3,4),(13.6829908479658,13.9346999333887,
14.9300356429165,15.9253713524443,16.920707061972,17.9160427714998,18.9113784810276,
19.9067141905553,19.9661761551454),.UNSPECIFIED.);
#789=B_SPLINE_CURVE_WITH_KNOTS('',3,(#35750,#35751,#35752,#35753,#35754,
#35755,#35756,#35757,#35758,#35759,#35760,#35761,#35762,#35763,#35764,#35765,
#35766,#35767,#35768,#35769,#35770,#35771),.UNSPECIFIED.,.F.,.F.,(4,3,3,
3,3,3,3,4),(-29.2243112993258,-28.8647355763052,-27.8693998667775,-26.8740641572497,
-25.8787284477219,-24.8833927381942,-23.8880570286664,-22.9411259921462),
 .UNSPECIFIED.);
#790=B_SPLINE_CURVE_WITH_KNOTS('',3,(#35772,#35773,#35774,#35775,#35776,
#35777,#35778,#35779,#35780,#35781,#35782,#35783,#35784,#35785,#35786,#35787,
#35788,#35789,#35790,#35791,#35792,#35793),.UNSPECIFIED.,.F.,.F.,(4,3,3,
3,3,3,3,4),(19.9661761551454,20.9020499000831,21.8973856096109,22.8927213191386,
23.8880570286664,24.8833927381942,25.8787284477219,26.2493614623249),
 .UNSPECIFIED.);
#791=B_SPLINE_CURVE_WITH_KNOTS('',3,(#35798,#35799,#35800,#35801,#35802,
#35803,#35804,#35805,#35806,#35807,#35808,#35809,#35810,#35811,#35812,#35813,
#35814,#35815,#35816,#35817,#35818,#35819),.UNSPECIFIED.,.F.,.F.,(4,3,3,
3,3,3,3,4),(-35.5074966065054,-34.8367498334718,-33.8414141239441,-32.8460784144163,
-31.8507427048885,-30.8554069953608,-29.860071285833,-29.2243112993258),
 .UNSPECIFIED.);
#792=B_SPLINE_CURVE_WITH_KNOTS('',3,(#35820,#35821,#35822,#35823,#35824,
#35825,#35826,#35827,#35828,#35829,#35830,#35831,#35832,#35833,#35834,#35835,
#35836,#35837,#35838,#35839,#35840,#35841),.UNSPECIFIED.,.F.,.F.,(4,3,3,
3,3,3,3,4),(26.2493614623249,26.8740641572497,27.8693998667775,28.8647355763052,
29.860071285833,30.8554069953608,31.8507427048885,32.5325467695045),
 .UNSPECIFIED.);
#793=B_SPLINE_CURVE_WITH_KNOTS('',3,(#35846,#35847,#35848,#35849,#35850,
#35851,#35852,#35853,#35854,#35855,#35856,#35857,#35858,#35859,#35860,#35861,
#35862,#35863,#35864,#35865,#35866,#35867),.UNSPECIFIED.,.F.,.F.,(4,3,3,
3,3,3,3,4),(-41.790681913685,-40.8087640906384,-39.8134283811107,-38.8180926715829,
-37.8227569620551,-36.8274212525274,-35.8320855429996,-35.5074966065054),
 .UNSPECIFIED.);
#794=B_SPLINE_CURVE_WITH_KNOTS('',3,(#35868,#35869,#35870,#35871,#35872,
#35873,#35874,#35875,#35876,#35877,#35878,#35879,#35880,#35881,#35882,#35883,
#35884,#35885,#35886,#35887,#35888,#35889),.UNSPECIFIED.,.F.,.F.,(4,3,3,
3,3,3,3,4),(32.5325467695045,32.8460784144163,33.8414141239441,34.8367498334718,
35.8320855429996,36.8274212525274,37.8227569620551,38.8157320766841),
 .UNSPECIFIED.);
#795=B_SPLINE_CURVE_WITH_KNOTS('',3,(#35894,#35895,#35896,#35897,#35898,
#35899,#35900,#35901,#35902,#35903,#35904,#35905,#35906,#35907,#35908,#35909,
#35910,#35911,#35912,#35913,#35914,#35915,#35916,#35917,#35918),
 .UNSPECIFIED.,.F.,.F.,(4,3,3,3,3,3,3,3,4),(-48.0738672208646,-47.7761140573328,
-46.780778347805,-45.7854426382773,-44.7901069287495,-43.7947712192217,
-42.799435509694,-41.8040998001662,-41.790681913685),.UNSPECIFIED.);
#796=B_SPLINE_CURVE_WITH_KNOTS('',3,(#35919,#35920,#35921,#35922,#35923,
#35924,#35925,#35926,#35927,#35928,#35929,#35930,#35931,#35932,#35933,#35934,
#35935,#35936,#35937,#35938,#35939,#35940,#35941,#35942,#35943),
 .UNSPECIFIED.,.F.,.F.,(4,3,3,3,3,3,3,3,4),(38.8157320766841,38.8180926715829,
39.8134283811107,40.8087640906384,41.8040998001662,42.799435509694,43.7947712192217,
44.7901069287495,45.0989173838637),.UNSPECIFIED.);
#797=B_SPLINE_CURVE_WITH_KNOTS('',3,(#35948,#35949,#35950,#35951,#35952,
#35953,#35954,#35955,#35956,#35957,#35958,#35959,#35960,#35961,#35962,#35963,
#35964,#35965,#35966,#35967,#35968,#35969),.UNSPECIFIED.,.F.,.F.,(4,3,3,
3,3,3,3,4),(-54.3570525280442,-53.7481283144994,-52.7527926049716,-51.7574568954439,
-50.7621211859161,-49.7667854763883,-48.7714497668606,-48.0738672208646),
 .UNSPECIFIED.);
#798=B_SPLINE_CURVE_WITH_KNOTS('',3,(#35970,#35971,#35972,#35973,#35974,
#35975,#35976,#35977,#35978,#35979,#35980,#35981,#35982,#35983,#35984,#35985,
#35986,#35987,#35988,#35989,#35990,#35991),.UNSPECIFIED.,.F.,.F.,(4,3,3,
3,3,3,3,4),(45.0989173838637,45.7854426382773,46.780778347805,47.7761140573328,
48.7714497668606,49.7667854763883,50.7621211859161,51.3821026910433),
 .UNSPECIFIED.);
#799=B_SPLINE_CURVE_WITH_KNOTS('',3,(#35996,#35997,#35998,#35999,#36000,
#36001,#36002,#36003,#36004,#36005,#36006,#36007,#36008,#36009,#36010,#36011,
#36012,#36013,#36014,#36015,#36016,#36017),.UNSPECIFIED.,.F.,.F.,(4,3,3,
3,3,3,3,4),(-60.6402378352238,-59.720142571666,-58.7248068621382,-57.7294711526105,
-56.7341354430827,-55.7387997335549,-54.7434640240272,-54.3570525280442),
 .UNSPECIFIED.);
#800=B_SPLINE_CURVE_WITH_KNOTS('',3,(#36018,#36019,#36020,#36021,#36022,
#36023,#36024,#36025,#36026,#36027,#36028,#36029,#36030,#36031,#36032,#36033,
#36034,#36035,#36036,#36037,#36038,#36039),.UNSPECIFIED.,.F.,.F.,(4,3,3,
3,3,3,3,4),(51.3821026910433,51.7574568954439,52.7527926049716,53.7481283144994,
54.7434640240272,55.7387997335549,56.7341354430827,57.6652879982229),
 .UNSPECIFIED.);
#801=B_SPLINE_CURVE_WITH_KNOTS('',3,(#36044,#36045,#36046,#36047,#36048,
#36049,#36050,#36051,#36052,#36053,#36054,#36055,#36056,#36057,#36058,#36059,
#36060,#36061,#36062,#36063,#36064,#36065,#36066,#36067,#36068),
 .UNSPECIFIED.,.F.,.F.,(4,3,3,3,3,3,3,3,4),(-66.9234231424034,-66.6874925383604,
-65.6921568288326,-64.6968211193048,-63.7014854097771,-62.7061497002493,
-61.7108139907215,-60.7154782811938,-60.6402378352238),.UNSPECIFIED.);
#802=B_SPLINE_CURVE_WITH_KNOTS('',3,(#36069,#36070,#36071,#36072,#36073,
#36074,#36075,#36076,#36077,#36078,#36079,#36080,#36081,#36082,#36083,#36084,
#36085,#36086,#36087,#36088,#36089,#36090,#36091,#36092,#36093),
 .UNSPECIFIED.,.F.,.F.,(4,3,3,3,3,3,3,3,4),(57.6652879982229,57.7294711526105,
58.7248068621382,59.720142571666,60.7154782811938,61.7108139907215,62.7061497002493,
63.7014854097771,63.9484733054025),.UNSPECIFIED.);
#803=B_SPLINE_CURVE_WITH_KNOTS('',3,(#36098,#36099,#36100,#36101,#36102,
#36103,#36104,#36105,#36106,#36107,#36108,#36109,#36110,#36111,#36112,#36113,
#36114,#36115,#36116,#36117,#36118,#36119),.UNSPECIFIED.,.F.,.F.,(4,3,3,
3,3,3,3,4),(-73.206608449583,-72.659506795527,-71.6641710859992,-70.6688353764714,
-69.6734996669437,-68.6781639574159,-67.6828282478881,-66.9234231424034),
 .UNSPECIFIED.);
#804=B_SPLINE_CURVE_WITH_KNOTS('',3,(#36120,#36121,#36122,#36123,#36124,
#36125,#36126,#36127,#36128,#36129,#36130,#36131,#36132,#36133,#36134,#36135,
#36136,#36137,#36138,#36139,#36140,#36141),.UNSPECIFIED.,.F.,.F.,(4,3,3,
3,3,3,3,4),(63.9484733054025,64.6968211193048,65.6921568288326,66.6874925383604,
67.6828282478881,68.6781639574159,69.6734996669437,70.2316586125821),
 .UNSPECIFIED.);
#805=B_SPLINE_CURVE_WITH_KNOTS('',3,(#36146,#36147,#36148,#36149,#36150,
#36151,#36152,#36153,#36154,#36155,#36156,#36157,#36158,#36159,#36160,#36161,
#36162,#36163,#36164,#36165,#36166,#36167),.UNSPECIFIED.,.F.,.F.,(4,3,3,
3,3,3,3,4),(-79.4897937567626,-78.6315210526936,-77.6361853431658,-76.640849633638,
-75.6455139241102,-74.6501782145825,-73.6548425050547,-73.206608449583),
 .UNSPECIFIED.);
#806=B_SPLINE_CURVE_WITH_KNOTS('',3,(#36168,#36169,#36170,#36171,#36172,
#36173,#36174,#36175,#36176,#36177,#36178,#36179,#36180,#36181,#36182,#36183,
#36184,#36185,#36186,#36187,#36188,#36189),.UNSPECIFIED.,.F.,.F.,(4,3,3,
3,3,3,3,4),(70.2316586125821,70.6688353764714,71.6641710859992,72.659506795527,
73.6548425050547,74.6501782145825,75.6455139241103,76.5148439197617),
 .UNSPECIFIED.);
#807=B_SPLINE_CURVE_WITH_KNOTS('',3,(#36194,#36195,#36196,#36197,#36198,
#36199,#36200,#36201,#36202,#36203,#36204,#36205,#36206,#36207,#36208,#36209,
#36210,#36211,#36212,#36213,#36214,#36215,#36216,#36217,#36218),
 .UNSPECIFIED.,.F.,.F.,(4,3,3,3,3,3,3,3,4),(-85.7729790639422,-85.5988710193879,
-84.6035353098602,-83.6081996003324,-82.6128638908046,-81.6175281812769,
-80.6221924717491,-79.6268567622213,-79.4897937567626),.UNSPECIFIED.);
#808=B_SPLINE_CURVE_WITH_KNOTS('',3,(#36219,#36220,#36221,#36222,#36223,
#36224,#36225,#36226,#36227,#36228,#36229,#36230,#36231,#36232,#36233,#36234,
#36235,#36236,#36237,#36238,#36239,#36240,#36241,#36242,#36243),
 .UNSPECIFIED.,.F.,.F.,(4,3,3,3,3,3,3,3,4),(76.5148439197617,76.640849633638,
77.6361853431658,78.6315210526936,79.6268567622213,80.6221924717491,81.6175281812769,
82.6128638908046,82.7980292269413),.UNSPECIFIED.);
#809=B_SPLINE_CURVE_WITH_KNOTS('',3,(#36248,#36249,#36250,#36251,#36252,
#36253,#36254,#36255,#36256,#36257,#36258,#36259,#36260,#36261,#36262,#36263,
#36264,#36265,#36266,#36267,#36268,#36269),.UNSPECIFIED.,.F.,.F.,(4,3,3,
3,3,3,3,4),(-92.0561643711218,-91.5708852765545,-90.5755495670268,-89.580213857499,
-88.5848781479712,-87.5895424384435,-86.5942067289157,-85.7729790639422),
 .UNSPECIFIED.);
#810=B_SPLINE_CURVE_WITH_KNOTS('',3,(#36270,#36271,#36272,#36273,#36274,
#36275,#36276,#36277,#36278,#36279,#36280,#36281,#36282,#36283,#36284,#36285,
#36286,#36287,#36288,#36289,#36290,#36291),.UNSPECIFIED.,.F.,.F.,(4,3,3,
3,3,3,3,4),(82.7980292269413,83.6081996003324,84.6035353098601,85.5988710193879,
86.5942067289157,87.5895424384435,88.5848781479712,89.0812145341209),
 .UNSPECIFIED.);
#811=B_SPLINE_CURVE_WITH_KNOTS('',3,(#36297,#36298,#36299,#36300,#36301,
#36302,#36303,#36304,#36305),.UNSPECIFIED.,.F.,.F.,(4,1,1,1,1,1,4),(97.3893722612836,
98.2105999262571,99.2059356357849,100.201271345313,101.19660705484,102.191942764368,
103.111352242327),.UNSPECIFIED.);
#812=B_SPLINE_CURVE_WITH_KNOTS('',3,(#36308,#36309,#36310,#36311,#36312,
#36313,#36314,#36315),.UNSPECIFIED.,.F.,.F.,(4,1,1,1,1,4),(97.3893722612836,
97.8883715846616,98.8837072941894,99.8790430037171,100.874378713245,101.869714422773),
 .UNSPECIFIED.);
#813=B_SPLINE_CURVE_WITH_KNOTS('',3,(#36320,#36321,#36322,#36323,#36324,
#36325,#36326,#36327,#36328,#36329,#36330),.UNSPECIFIED.,.F.,.F.,(4,1,1,
1,1,1,1,1,4),(91.106186954104,91.2432499595627,92.2385856690905,93.2339213786183,
94.229257088146,95.2245927976738,96.2199285072016,97.2152642167293,97.3893722612836),
 .UNSPECIFIED.);
#814=B_SPLINE_CURVE_WITH_KNOTS('',3,(#36331,#36332,#36333,#36334,#36335,
#36336,#36337,#36338,#36339,#36340),.UNSPECIFIED.,.F.,.F.,(4,1,1,1,1,1,
1,4),(91.106186954104,91.916357327495,92.9116930370228,93.9070287465505,
94.9023644560783,95.8977001656061,96.8930358751338,97.3893722612836),
 .UNSPECIFIED.);
#815=B_SPLINE_CURVE_WITH_KNOTS('',3,(#36345,#36346,#36347,#36348,#36349,
#36350,#36351,#36352,#36353,#36354),.UNSPECIFIED.,.F.,.F.,(4,1,1,1,1,1,
1,4),(84.8230016469244,85.2712357023961,86.2665714119239,87.2619071214517,
88.2572428309794,89.2525785405072,90.247914250035,91.106186954104),
 .UNSPECIFIED.);
#816=B_SPLINE_CURVE_WITH_KNOTS('',3,(#36355,#36356,#36357,#36358,#36359,
#36360,#36361,#36362,#36363,#36364,#36365),.UNSPECIFIED.,.F.,.F.,(4,1,1,
1,1,1,1,1,4),(84.8230016469244,84.9490073608006,85.9443430703284,86.9396787798562,
87.9350144893839,88.9303501989117,89.9256859084395,90.9210216179672,91.106186954104),
 .UNSPECIFIED.);
#817=B_SPLINE_CURVE_WITH_KNOTS('',3,(#36370,#36371,#36372,#36373,#36374,
#36375,#36376,#36377,#36378,#36379),.UNSPECIFIED.,.F.,.F.,(4,1,1,1,1,1,
1,4),(78.5398163397448,79.2992214452295,80.2945571547573,81.2898928642851,
82.2852285738128,83.2805642833406,84.2758999928684,84.8230016469244),
 .UNSPECIFIED.);
#818=B_SPLINE_CURVE_WITH_KNOTS('',3,(#36380,#36381,#36382,#36383,#36384,
#36385,#36386,#36387,#36388,#36389),.UNSPECIFIED.,.F.,.F.,(4,1,1,1,1,1,
1,4),(78.5398163397448,78.976993103634,79.9723288131618,80.9676645226896,
81.9630002322173,82.9583359417451,83.9536716512729,84.8230016469244),
 .UNSPECIFIED.);
#819=B_SPLINE_CURVE_WITH_KNOTS('',3,(#36394,#36395,#36396,#36397,#36398,
#36399,#36400,#36401,#36402,#36403,#36404),.UNSPECIFIED.,.F.,.F.,(4,1,1,
1,1,1,1,1,4),(72.2566310325652,72.3318714785352,73.3272071880629,74.3225428975907,
75.3178786071185,76.3132143166462,77.308550026174,78.3038857357018,78.5398163397448),
 .UNSPECIFIED.);
#820=B_SPLINE_CURVE_WITH_KNOTS('',3,(#36405,#36406,#36407,#36408,#36409,
#36410,#36411,#36412,#36413,#36414),.UNSPECIFIED.,.F.,.F.,(4,1,1,1,1,1,
1,4),(72.2566310325652,73.0049788464674,74.0003145559952,74.995650265523,
75.9909859750507,76.9863216845785,77.9816573941063,78.5398163397448),
 .UNSPECIFIED.);
#821=B_SPLINE_CURVE_WITH_KNOTS('',3,(#36419,#36420,#36421,#36422,#36423,
#36424,#36425,#36426,#36427,#36428),.UNSPECIFIED.,.F.,.F.,(4,1,1,1,1,1,
1,4),(65.9734457253856,66.3598572213686,67.3551929308963,68.3505286404241,
69.3458643499519,70.3412000594796,71.3365357690074,72.2566310325652),
 .UNSPECIFIED.);
#822=B_SPLINE_CURVE_WITH_KNOTS('',3,(#36429,#36430,#36431,#36432,#36433,
#36434,#36435,#36436,#36437,#36438,#36439),.UNSPECIFIED.,.F.,.F.,(4,1,1,
1,1,1,1,1,4),(65.9734457253856,66.0376288797731,67.0329645893008,68.0283002988286,
69.0236360083564,70.0189717178841,71.0143074274119,72.0096431369397,72.2566310325652),
 .UNSPECIFIED.);
#823=B_SPLINE_CURVE_WITH_KNOTS('',3,(#36444,#36445,#36446,#36447,#36448,
#36449,#36450,#36451,#36452,#36453),.UNSPECIFIED.,.F.,.F.,(4,1,1,1,1,1,
1,4),(59.690260418206,60.387842964202,61.3831786737297,62.3785143832575,
63.3738500927853,64.369185802313,65.3645215118408,65.9734457253856),
 .UNSPECIFIED.);
#824=B_SPLINE_CURVE_WITH_KNOTS('',3,(#36454,#36455,#36456,#36457,#36458,
#36459,#36460,#36461,#36462,#36463),.UNSPECIFIED.,.F.,.F.,(4,1,1,1,1,1,
1,4),(59.690260418206,60.0656146226065,61.0609503321342,62.056286041662,
63.0516217511898,64.0469574607175,65.0422931702453,65.9734457253856),
 .UNSPECIFIED.);
#825=B_SPLINE_CURVE_WITH_KNOTS('',3,(#36468,#36469,#36470,#36471,#36472,
#36473,#36474,#36475,#36476,#36477,#36478),.UNSPECIFIED.,.F.,.F.,(4,1,1,
1,1,1,1,1,4),(53.4070751110264,53.4204929975076,54.4158287070354,55.4111644165631,
56.4065001260909,57.4018358356187,58.3971715451464,59.3925072546742,59.690260418206),
 .UNSPECIFIED.);
#826=B_SPLINE_CURVE_WITH_KNOTS('',3,(#36479,#36480,#36481,#36482,#36483,
#36484,#36485,#36486,#36487,#36488),.UNSPECIFIED.,.F.,.F.,(4,1,1,1,1,1,
1,4),(53.4070751110264,54.0936003654399,55.0889360749676,56.0842717844954,
57.0796074940232,58.0749432035509,59.0702789130787,59.690260418206),
 .UNSPECIFIED.);
#827=B_SPLINE_CURVE_WITH_KNOTS('',3,(#36493,#36494,#36495,#36496,#36497,
#36498,#36499,#36500,#36501,#36502),.UNSPECIFIED.,.F.,.F.,(4,1,1,1,1,1,
1,4),(47.1238898038469,47.448478740341,48.4438144498688,49.4391501593965,
50.4344858689243,51.4298215784521,52.4251572879798,53.4070751110264),
 .UNSPECIFIED.);
#828=B_SPLINE_CURVE_WITH_KNOTS('',3,(#36503,#36504,#36505,#36506,#36507,
#36508,#36509,#36510,#36511,#36512,#36513),.UNSPECIFIED.,.F.,.F.,(4,1,1,
1,1,1,1,1,4),(47.1238898038468,47.1262503987455,48.1215861082733,49.116921817801,
50.1122575273288,51.1075932368566,52.1029289463843,53.0982646559121,53.4070751110264),
 .UNSPECIFIED.);
#829=B_SPLINE_CURVE_WITH_KNOTS('',3,(#36518,#36519,#36520,#36521,#36522,
#36523,#36524,#36525,#36526,#36527),.UNSPECIFIED.,.F.,.F.,(4,1,1,1,1,1,
1,4),(40.8407044966673,41.4764644831744,42.4718001927022,43.4671359022299,
44.4624716117577,45.4578073212855,46.4531430308133,47.1238898038469),
 .UNSPECIFIED.);
#830=B_SPLINE_CURVE_WITH_KNOTS('',3,(#36528,#36529,#36530,#36531,#36532,
#36533,#36534,#36535,#36536,#36537),.UNSPECIFIED.,.F.,.F.,(4,1,1,1,1,1,
1,4),(40.8407044966672,41.1542361415789,42.1495718511067,43.1449075606344,
44.1402432701622,45.13557897969,46.1309146892177,47.1238898038468),
 .UNSPECIFIED.);
#831=B_SPLINE_CURVE_WITH_KNOTS('',3,(#36542,#36543,#36544,#36545,#36546,
#36547,#36548,#36549,#36550,#36551),.UNSPECIFIED.,.F.,.F.,(4,1,1,1,1,1,
1,4),(34.5575191894877,35.5044502260078,36.4997859355356,37.4951216450633,
38.4904573545911,39.4857930641189,40.4811287736466,40.8407044966673),
 .UNSPECIFIED.);
#832=B_SPLINE_CURVE_WITH_KNOTS('',3,(#36552,#36553,#36554,#36555,#36556,
#36557,#36558,#36559,#36560,#36561),.UNSPECIFIED.,.F.,.F.,(4,1,1,1,1,1,
1,4),(34.5575191894876,35.1822218844123,36.1775575939401,37.1728933034678,
38.1682290129956,39.1635647225234,40.1589004320511,40.8407044966672),
 .UNSPECIFIED.);
#833=B_SPLINE_CURVE_WITH_KNOTS('',3,(#36566,#36567,#36568,#36569,#36570,
#36571,#36572,#36573,#36574,#36575,#36576),.UNSPECIFIED.,.F.,.F.,(4,1,1,
1,1,1,1,1,4),(28.2743338823081,28.5371002593134,29.5324359688412,30.527771678369,
31.5231073878967,32.5184430974245,33.5137788069523,34.50911451648,34.5575191894877),
 .UNSPECIFIED.);
#834=B_SPLINE_CURVE_WITH_KNOTS('',3,(#36577,#36578,#36579,#36580,#36581,
#36582,#36583,#36584,#36585,#36586),.UNSPECIFIED.,.F.,.F.,(4,1,1,1,1,1,
1,4),(28.2743338823081,29.2102076272457,30.2055433367735,31.2008790463012,
32.196214755829,33.1915504653568,34.1868861748845,34.5575191894876),
 .UNSPECIFIED.);
#835=B_SPLINE_CURVE_WITH_KNOTS('',3,(#36591,#36592,#36593,#36594,#36595,
#36596,#36597,#36598,#36599,#36600),.UNSPECIFIED.,.F.,.F.,(4,1,1,1,1,1,
1,4),(21.9911485751285,22.5650860021468,23.5604217116746,24.5557574212024,
25.5510931307301,26.5464288402579,27.5417645497857,28.2743338823081),
 .UNSPECIFIED.);
#836=B_SPLINE_CURVE_WITH_KNOTS('',3,(#36601,#36602,#36603,#36604,#36605,
#36606,#36607,#36608,#36609,#36610,#36611),.UNSPECIFIED.,.F.,.F.,(4,1,1,
1,1,1,1,1,4),(21.9911485751285,22.2428576605513,23.2381933700791,24.2335290796069,
25.2288647891346,26.2242004986624,27.2195362081902,28.2148719177179,28.2743338823081),
 .UNSPECIFIED.);
#837=B_SPLINE_CURVE_WITH_KNOTS('',3,(#36616,#36617,#36618,#36619,#36620,
#36621,#36622,#36623,#36624,#36625),.UNSPECIFIED.,.F.,.F.,(4,1,1,1,1,1,
1,4),(15.7079632679489,16.5930717449802,17.588407454508,18.5837431640358,
19.5790788735635,20.5744145830913,21.5697502926191,21.9911485751285),
 .UNSPECIFIED.);
#838=B_SPLINE_CURVE_WITH_KNOTS('',3,(#36626,#36627,#36628,#36629,#36630,
#36631,#36632,#36633,#36634,#36635),.UNSPECIFIED.,.F.,.F.,(4,1,1,1,1,1,
1,4),(15.7079632679489,16.2708434033847,17.2661791129125,18.2615148224403,
19.256850531968,20.2521862414958,21.2475219510236,21.9911485751285),
 .UNSPECIFIED.);
#839=B_SPLINE_CURVE_WITH_KNOTS('',3,(#37025,#37026,#37027,#37028,#37029,
#37030,#37031,#37032,#37033,#37034,#37035,#37036,#37037,#37038,#37039,#37040,
#37041,#37042,#37043,#37044,#37045,#37046,#37047,#37048,#37049,#37050,#37051,
#37052,#37053,#37054,#37055,#37056,#37057,#37058,#37059,#37060,#37061,#37062,
#37063,#37064,#37065,#37066,#37067,#37068,#37069,#37070,#37071,#37072,#37073,
#37074,#37075,#37076,#37077,#37078,#37079,#37080,#37081,#37082,#37083,#37084,
#37085,#37086,#37087,#37088,#37089,#37090,#37091,#37092,#37093,#37094,#37095,
#37096,#37097,#37098,#37099,#37100,#37101,#37102,#37103,#37104,#37105,#37106,
#37107,#37108,#37109,#37110,#37111,#37112),.UNSPECIFIED.,.F.,.F.,(4,3,3,
3,3,3,3,3,3,3,3,3,3,3,3,3,3,3,3,3,3,3,3,3,3,3,3,3,3,4),(-0.461788964899778,
-0.4432234502138,-0.417585071690447,-0.404676823606039,-0.398380133623887,
-0.393259612278708,-0.367874849545492,-0.348272131144797,-0.338456418860554,
-0.332916476029383,-0.308151864898805,-0.283877174259086,-0.260161043087549,
-0.251332965374558,-0.246977223747103,-0.243306514944723,-0.219829616972232,
-0.211053102339927,-0.187088418858572,-0.163702366501251,-0.158787258719064,
-0.135433187942531,-0.112095172587591,-0.0891454130303583,-0.0803315821691377,
-0.0766175667602699,-0.0541537505784823,-0.0320531226257585,-0.0106595864360154,
0.),.UNSPECIFIED.);
#840=B_SPLINE_CURVE_WITH_KNOTS('',3,(#37113,#37114,#37115,#37116,#37117,
#37118,#37119,#37120,#37121,#37122),.UNSPECIFIED.,.F.,.F.,(4,3,3,4),(89.0812145341209,
89.580213857499,90.5755495670267,91.4949590449857),.UNSPECIFIED.);
#841=B_SPLINE_CURVE_WITH_KNOTS('',3,(#37124,#37125,#37126,#37127,#37128,
#37129,#37130,#37131,#37132,#37133,#37134,#37135,#37136,#37137,#37138,#37139,
#37140,#37141,#37142,#37143,#37144,#37145,#37146,#37147,#37148,#37149,#37150,
#37151,#37152,#37153,#37154,#37155,#37156,#37157,#37158,#37159,#37160,#37161,
#37162,#37163,#37164,#37165,#37166,#37167,#37168,#37169,#37170,#37171,#37172,
#37173,#37174,#37175,#37176,#37177,#37178,#37179,#37180,#37181,#37182,#37183,
#37184,#37185,#37186,#37187,#37188,#37189,#37190,#37191,#37192,#37193,#37194,
#37195,#37196,#37197,#37198,#37199,#37200,#37201,#37202,#37203,#37204,#37205,
#37206,#37207,#37208),.UNSPECIFIED.,.F.,.F.,(4,3,3,3,3,3,3,3,3,3,3,3,3,
3,3,3,3,3,3,3,3,3,3,3,3,3,3,3,4),(-0.463803050843711,-0.448429413206914,
-0.426704171981601,-0.414159993364273,-0.409718066359999,-0.387136470680841,
-0.368120384440548,-0.35895595361815,-0.354767190879561,-0.331504579574296,
-0.307380379870345,-0.289287230092382,-0.275717367758909,-0.271450226768227,
-0.267796738492813,-0.243369230116364,-0.235007780758492,-0.211413020390669,
-0.187330446081715,-0.181489281437917,-0.157060938111767,-0.132145865675509,
-0.107037279266715,-0.0963831544778031,-0.0910163492829886,-0.0652783368980751,
-0.0394980984327342,-0.0142604401573251,0.),.UNSPECIFIED.);
#842=B_SPLINE_CURVE_WITH_KNOTS('',3,(#37209,#37210,#37211,#37212,#37213,
#37214,#37215,#37216,#37217),.UNSPECIFIED.,.F.,.F.,(4,1,1,1,1,1,4),(10.374755377787,
11.2941648557459,12.2895005652737,13.2848362748014,14.2801719843292,15.275507693857,
15.7079632679489),.UNSPECIFIED.);
#843=B_SPLINE_CURVE_WITH_KNOTS('',3,(#37223,#37224,#37225,#37226,#37227,
#37228,#37229,#37230,#37231,#37232,#37233,#37234,#37235,#37236,#37237,#37238,
#37239,#37240,#37241,#37242,#37243,#37244,#37245,#37246,#37247,#37248,#37249,
#37250,#37251,#37252,#37253,#37254,#37255,#37256,#37257,#37258,#37259,#37260,
#37261,#37262,#37263,#37264,#37265,#37266,#37267,#37268,#37269,#37270,#37271,
#37272,#37273,#37274,#37275,#37276,#37277,#37278,#37279,#37280,#37281,#37282,
#37283,#37284,#37285,#37286,#37287,#37288,#37289,#37290,#37291,#37292,#37293,
#37294,#37295,#37296,#37297,#37298,#37299,#37300,#37301,#37302,#37303,#37304,
#37305,#37306,#37307,#37308,#37309,#37310),.UNSPECIFIED.,.F.,.F.,(4,3,3,
3,3,3,3,3,3,3,3,3,3,3,3,3,3,3,3,3,3,3,3,3,3,3,3,3,3,4),(-0.461788964899765,
-0.443223450213792,-0.417585071143145,-0.404676823092943,-0.398380110287486,
-0.393259604558869,-0.367874841639472,-0.348272124227028,-0.338456405730752,
-0.332916474245839,-0.308151862176156,-0.283877172217097,-0.260161025980822,
-0.251332920274659,-0.246977167765169,-0.243306502630573,-0.219829594194119,
-0.211053102339921,-0.187088411880509,-0.163702360395445,-0.158787259103022,
-0.135433184446935,-0.112095174888583,-0.0891454298609094,-0.0803315842997371,
-0.0766175679727495,-0.0541537625388748,-0.0320531510297545,-0.010659635642814,
0.),.UNSPECIFIED.);
#844=B_SPLINE_CURVE_WITH_KNOTS('',3,(#37313,#37314,#37315,#37316,#37317,
#37318,#37319,#37320),.UNSPECIFIED.,.F.,.F.,(4,1,1,1,1,4),(11.6163931973414,
12.6117289068692,13.6070646163969,14.6024003259247,15.5977360354525,15.7079632679489),
 .UNSPECIFIED.);
#845=B_SPLINE_CURVE_WITH_KNOTS('',3,(#37710,#37711,#37712,#37713,#37714,
#37715,#37716,#37717,#37718,#37719,#37720,#37721,#37722,#37723,#37724,#37725,
#37726,#37727,#37728,#37729,#37730,#37731,#37732,#37733,#37734,#37735,#37736,
#37737,#37738,#37739,#37740,#37741,#37742,#37743,#37744,#37745,#37746,#37747,
#37748,#37749,#37750,#37751,#37752,#37753,#37754,#37755,#37756,#37757,#37758,
#37759,#37760,#37761,#37762,#37763,#37764,#37765,#37766,#37767,#37768,#37769,
#37770,#37771,#37772,#37773,#37774,#37775,#37776,#37777,#37778,#37779,#37780,
#37781,#37782,#37783,#37784,#37785,#37786,#37787,#37788,#37789,#37790,#37791,
#37792,#37793,#37794),.UNSPECIFIED.,.F.,.F.,(4,3,3,3,3,3,3,3,3,3,3,3,3,
3,3,3,3,3,3,3,3,3,3,3,3,3,3,3,4),(-0.463803050843705,-0.448429413206907,
-0.42670415944794,-0.4141599708977,-0.409718048450771,-0.387136443589144,
-0.368120360735312,-0.358955917726794,-0.354767147726934,-0.331504528371831,
-0.307380341468495,-0.289287201290993,-0.275717346157866,-0.271450058108256,
-0.267796704376614,-0.243369196611869,-0.235007780758486,-0.211413015229316,
-0.187330434823406,-0.181489285380682,-0.157060936178603,-0.132145857977694,
-0.107037270590661,-0.0963831412843047,-0.0910163503959406,-0.0652783344338678,
-0.0394980989815758,-0.0142604566308707,0.),.UNSPECIFIED.);
#846=B_SPLINE_CURVE_WITH_KNOTS('',3,(#37795,#37796,#37797,#37798,#37799,
#37800,#37801),.UNSPECIFIED.,.F.,.F.,(4,3,4),(-93.5615566956101,-92.5662209860823,
-92.0561643711218),.UNSPECIFIED.);
#847=CONICAL_SURFACE('',#17255,47.75,0.785398163397447);
#848=CONICAL_SURFACE('',#17266,47.75,0.785398163397447);
#849=CONICAL_SURFACE('',#17279,2.8,0.785398163397449);
#850=CONICAL_SURFACE('',#17291,47.8232233047034,0.392699081698724);
#851=CONICAL_SURFACE('',#17294,47.6,0.785398163397448);
#852=CONICAL_SURFACE('',#17297,11.25,0.785398163397446);
#853=CONICAL_SURFACE('',#17301,47.1267766952966,1.17809724509617);
#854=CONICAL_SURFACE('',#17307,11.3,0.785398163397444);
#855=CONICAL_SURFACE('',#17328,53.25,0.785398163397446);
#856=CONICAL_SURFACE('',#17334,53.25,0.785398163397446);
#857=CONICAL_SURFACE('',#17341,0.950000000000001,0.785398163397444);
#858=CONICAL_SURFACE('',#17350,0.950000000000001,0.785398163397445);
#859=CONICAL_SURFACE('',#17353,0.950000000000004,0.785398163397449);
#860=CONICAL_SURFACE('',#17364,53.25,0.785398163397446);
#861=CONICAL_SURFACE('',#17371,53.25,0.785398163397446);
#862=CONICAL_SURFACE('',#17374,53.25,0.785398163397446);
#863=CONICAL_SURFACE('',#17381,53.25,0.785398163397455);
#864=CONICAL_SURFACE('',#17388,53.25,0.785398163397446);
#865=CONICAL_SURFACE('',#17395,53.25,0.785398163397446);
#866=CONICAL_SURFACE('',#17402,53.25,0.785398163397446);
#867=CONICAL_SURFACE('',#17409,53.25,0.785398163397446);
#868=CONICAL_SURFACE('',#17416,53.25,0.785398163397446);
#869=CONICAL_SURFACE('',#17423,53.25,0.785398163397446);
#870=CONICAL_SURFACE('',#17429,0.950000000000002,0.785398163397447);
#871=CONICAL_SURFACE('',#17432,53.25,0.785398163397437);
#872=CONICAL_SURFACE('',#17435,53.25,0.785398163397455);
#873=CONICAL_SURFACE('',#17438,53.25,0.785398163397437);
#874=CONICAL_SURFACE('',#17606,0.950000000000002,0.785398163397447);
#875=CONICAL_SURFACE('',#17612,0.950000000000002,0.785398163397446);
#876=CONICAL_SURFACE('',#17618,0.950000000000005,0.785398163397452);
#877=CONICAL_SURFACE('',#17626,53.25,0.785398163397446);
#878=CONICAL_SURFACE('',#17629,53.25,0.785398163397437);
#879=CONICAL_SURFACE('',#17635,53.25,0.785398163397446);
#880=CONICAL_SURFACE('',#17641,53.25,0.785398163397446);
#881=CONICAL_SURFACE('',#17647,53.25,0.785398163397446);
#882=CONICAL_SURFACE('',#17653,53.25,0.785398163397455);
#883=CONICAL_SURFACE('',#17659,53.25,0.785398163397437);
#884=CONICAL_SURFACE('',#17664,53.25,0.785398163397437);
#885=CONICAL_SURFACE('',#17666,53.25,0.785398163397446);
#886=CONICAL_SURFACE('',#17668,53.25,0.785398163397437);
#887=CONICAL_SURFACE('',#17677,0.950000000000005,0.785398163397451);
#888=CONICAL_SURFACE('',#17679,0.950000000000004,0.78539816339745);
#889=CONICAL_SURFACE('',#17681,0.950000000000002,0.785398163397445);
#890=CONICAL_SURFACE('',#17683,0.950000000000003,0.785398163397449);
#891=CONICAL_SURFACE('',#17685,0.950000000000004,0.78539816339745);
#892=CONICAL_SURFACE('',#17700,0.950000000000005,0.785398163397451);
#893=CONICAL_SURFACE('',#17705,53.25,0.785398163397437);
#894=CONICAL_SURFACE('',#17708,0.950000000000001,0.785398163397444);
#895=CONICAL_SURFACE('',#17714,0.950000000000003,0.785398163397448);
#896=CONICAL_SURFACE('',#17720,0.950000000000003,0.785398163397447);
#897=CONICAL_SURFACE('',#17728,53.25,0.785398163397437);
#898=CONICAL_SURFACE('',#17731,53.25,0.785398163397437);
#899=CONICAL_SURFACE('',#17737,53.25,0.785398163397446);
#900=CONICAL_SURFACE('',#17743,53.25,0.785398163397446);
#901=CONICAL_SURFACE('',#17749,53.25,0.785398163397446);
#902=CONICAL_SURFACE('',#17755,53.25,0.785398163397446);
#903=CONICAL_SURFACE('',#17760,53.25,0.785398163397446);
#904=CONICAL_SURFACE('',#17762,53.25,0.785398163397437);
#905=CONICAL_SURFACE('',#17764,53.25,0.785398163397437);
#906=CONICAL_SURFACE('',#17775,0.950000000000002,0.785398163397446);
#907=CONICAL_SURFACE('',#17777,0.950000000000002,0.785398163397447);
#908=CONICAL_SURFACE('',#17779,0.950000000000003,0.785398163397448);
#909=CONICAL_SURFACE('',#17781,0.950000000000001,0.785398163397444);
#910=CONICAL_SURFACE('',#17794,0.950000000000002,0.785398163397447);
#911=CONICAL_SURFACE('',#17800,0.950000000000004,0.78539816339745);
#912=CONICAL_SURFACE('',#17806,0.950000000000003,0.785398163397449);
#913=CONICAL_SURFACE('',#17812,0.950000000000002,0.785398163397445);
#914=CONICAL_SURFACE('',#17818,0.950000000000004,0.78539816339745);
#915=CONICAL_SURFACE('',#17826,53.25,0.785398163397446);
#916=CONICAL_SURFACE('',#17829,53.25,0.785398163397446);
#917=CONICAL_SURFACE('',#17835,53.25,0.785398163397446);
#918=CONICAL_SURFACE('',#17841,53.25,0.785398163397446);
#919=CONICAL_SURFACE('',#17847,53.25,0.785398163397446);
#920=CONICAL_SURFACE('',#17852,53.25,0.785398163397446);
#921=CONICAL_SURFACE('',#17854,53.25,0.785398163397446);
#922=CONICAL_SURFACE('',#17856,53.25,0.785398163397455);
#923=CONICAL_SURFACE('',#17858,53.25,0.785398163397446);
#924=CONICAL_SURFACE('',#17860,53.25,0.785398163397446);
#925=CONICAL_SURFACE('',#17873,0.950000000000003,0.785398163397447);
#926=CONICAL_SURFACE('',#17875,0.950000000000005,0.785398163397452);
#927=CONICAL_SURFACE('',#17877,0.950000000000002,0.785398163397446);
#928=CONICAL_SURFACE('',#17888,0.950000000000001,0.785398163397445);
#929=CONICAL_SURFACE('',#17893,53.25,0.785398163397437);
#930=CONICAL_SURFACE('',#17896,0.950000000000003,0.785398163397449);
#931=CONICAL_SURFACE('',#17902,0.950000000000001,0.785398163397444);
#932=CONICAL_SURFACE('',#17908,0.950000000000004,0.785398163397449);
#933=CONICAL_SURFACE('',#17914,0.950000000000004,0.78539816339745);
#934=CONICAL_SURFACE('',#17920,0.950000000000001,0.785398163397444);
#935=CONICAL_SURFACE('',#17928,53.25,0.785398163397446);
#936=CONICAL_SURFACE('',#17931,53.25,0.785398163397437);
#937=CONICAL_SURFACE('',#17937,53.25,0.785398163397446);
#938=CONICAL_SURFACE('',#17943,53.25,0.785398163397455);
#939=CONICAL_SURFACE('',#17948,53.25,0.785398163397455);
#940=CONICAL_SURFACE('',#17950,53.25,0.785398163397437);
#941=CONICAL_SURFACE('',#17952,53.25,0.785398163397437);
#942=CONICAL_SURFACE('',#17954,53.25,0.785398163397446);
#943=CONICAL_SURFACE('',#17956,53.25,0.785398163397455);
#944=CONICAL_SURFACE('',#17971,0.950000000000003,0.785398163397448);
#945=CONICAL_SURFACE('',#17973,0.950000000000001,0.785398163397445);
#946=CONICAL_SURFACE('',#17982,0.950000000000002,0.785398163397446);
#947=CONICAL_SURFACE('',#17988,0.950000000000004,0.78539816339745);
#948=CONICAL_SURFACE('',#17994,0.950000000000002,0.785398163397447);
#949=CONICAL_SURFACE('',#18000,0.950000000000002,0.785398163397445);
#950=CONICAL_SURFACE('',#18006,0.950000000000001,0.785398163397444);
#951=CONICAL_SURFACE('',#18012,0.950000000000004,0.78539816339745);
#952=CONICAL_SURFACE('',#18018,0.950000000000004,0.78539816339745);
#953=CONICAL_SURFACE('',#18026,53.25,0.785398163397437);
#954=CONICAL_SURFACE('',#18029,53.25,0.785398163397446);
#955=CONICAL_SURFACE('',#18035,53.25,0.785398163397446);
#956=CONICAL_SURFACE('',#18040,53.25,0.785398163397446);
#957=CONICAL_SURFACE('',#18042,53.25,0.785398163397446);
#958=CONICAL_SURFACE('',#18044,53.25,0.785398163397437);
#959=CONICAL_SURFACE('',#18046,53.25,0.785398163397446);
#960=CONICAL_SURFACE('',#18048,53.25,0.785398163397437);
#961=CONICAL_SURFACE('',#18050,53.25,0.785398163397446);
#962=CONICAL_SURFACE('',#18052,53.25,0.785398163397446);
#963=CONICAL_SURFACE('',#18069,0.950000000000002,0.785398163397447);
#964=CONICAL_SURFACE('',#18076,0.950000000000001,0.785398163397444);
#965=CONICAL_SURFACE('',#18082,0.950000000000003,0.785398163397448);
#966=CONICAL_SURFACE('',#18088,0.950000000000003,0.785398163397447);
#967=CONICAL_SURFACE('',#18094,0.950000000000002,0.785398163397446);
#968=CONICAL_SURFACE('',#18100,0.950000000000005,0.785398163397452);
#969=CONICAL_SURFACE('',#18106,0.950000000000004,0.78539816339745);
#970=CONICAL_SURFACE('',#18112,0.950000000000002,0.785398163397445);
#971=CONICAL_SURFACE('',#18118,0.950000000000003,0.785398163397449);
#972=CONICAL_SURFACE('',#18126,53.25,0.785398163397455);
#973=CONICAL_SURFACE('',#18129,53.25,0.785398163397446);
#974=CONICAL_SURFACE('',#18134,53.25,0.785398163397437);
#975=CONICAL_SURFACE('',#18136,53.25,0.785398163397437);
#976=CONICAL_SURFACE('',#18138,53.25,0.785398163397446);
#977=CONICAL_SURFACE('',#18140,53.25,0.785398163397437);
#978=CONICAL_SURFACE('',#18142,53.25,0.785398163397446);
#979=CONICAL_SURFACE('',#18144,53.25,0.785398163397446);
#980=CONICAL_SURFACE('',#18146,53.25,0.785398163397446);
#981=CONICAL_SURFACE('',#18148,53.25,0.785398163397446);
#982=CONICAL_SURFACE('',#18170,53.25,0.785398163397446);
#983=CONICAL_SURFACE('',#18176,53.25,0.785398163397446);
#984=CONICAL_SURFACE('',#18182,53.25,0.785398163397446);
#985=CONICAL_SURFACE('',#18188,53.25,0.785398163397446);
#986=CONICAL_SURFACE('',#18194,53.25,0.785398163397446);
#987=CONICAL_SURFACE('',#18200,53.25,0.785398163397437);
#988=CONICAL_SURFACE('',#18206,53.25,0.785398163397446);
#989=CONICAL_SURFACE('',#18212,53.25,0.785398163397446);
#990=CONICAL_SURFACE('',#18218,53.25,0.785398163397446);
#991=CONICAL_SURFACE('',#18226,0.950000000000001,0.785398163397444);
#992=CONICAL_SURFACE('',#18228,0.950000000000004,0.78539816339745);
#993=CONICAL_SURFACE('',#18230,0.950000000000003,0.785398163397449);
#994=CONICAL_SURFACE('',#18232,0.950000000000002,0.785398163397445);
#995=CONICAL_SURFACE('',#18234,0.950000000000004,0.78539816339745);
#996=CONICAL_SURFACE('',#18236,0.950000000000005,0.785398163397452);
#997=CONICAL_SURFACE('',#18238,0.950000000000002,0.785398163397446);
#998=CONICAL_SURFACE('',#18240,0.950000000000003,0.785398163397447);
#999=CONICAL_SURFACE('',#18242,0.950000000000003,0.785398163397448);
#1000=CONICAL_SURFACE('',#18260,49.75,0.785398163397446);
#1001=CONICAL_SURFACE('',#18265,0.950000000000004,0.78539816339745);
#1002=CONICAL_SURFACE('',#18267,0.950000000000004,0.78539816339745);
#1003=CONICAL_SURFACE('',#18269,0.950000000000001,0.785398163397444);
#1004=CONICAL_SURFACE('',#18271,0.950000000000001,0.785398163397445);
#1005=CONICAL_SURFACE('',#18273,0.950000000000002,0.785398163397447);
#1006=CONICAL_SURFACE('',#18275,0.950000000000004,0.78539816339745);
#1007=CONICAL_SURFACE('',#18277,0.950000000000002,0.785398163397446);
#1008=CONICAL_SURFACE('',#18279,0.950000000000002,0.785398163397447);
#1009=CONICAL_SURFACE('',#18303,53.25,0.785398163397437);
#1010=CONICAL_SURFACE('',#18309,53.25,0.785398163397446);
#1011=CONICAL_SURFACE('',#18315,53.25,0.785398163397437);
#1012=CONICAL_SURFACE('',#18321,53.25,0.785398163397455);
#1013=CONICAL_SURFACE('',#18327,53.25,0.785398163397446);
#1014=CONICAL_SURFACE('',#18333,53.25,0.785398163397455);
#1015=CONICAL_SURFACE('',#18336,52.6267766952966,1.17809724509617);
#1016=CONICAL_SURFACE('',#18341,53.1,0.785398163397448);
#1017=CONICAL_SURFACE('',#18443,12.7,0.785398163397448);
#1018=CONICAL_SURFACE('',#18455,12.7,0.785398163397448);
#1019=CONICAL_SURFACE('',#18459,12.7,0.785398163397448);
#1020=CONICAL_SURFACE('',#18463,12.7,0.785398163397448);
#1021=CONICAL_SURFACE('',#18467,12.7,0.785398163397448);
#1022=CONICAL_SURFACE('',#18471,50.8,0.785398163397444);
#1023=CONICAL_SURFACE('',#18586,1.5,0.785398163397448);
#1024=CONICAL_SURFACE('',#18588,1.5,0.785398163397448);
#1025=CONICAL_SURFACE('',#18590,1.5,0.785398163397448);
#1026=CONICAL_SURFACE('',#18592,1.5,0.785398163397448);
#1027=CONICAL_SURFACE('',#18594,1.5,0.785398163397448);
#1028=CONICAL_SURFACE('',#18638,13.3,0.785398163397449);
#1029=CONICAL_SURFACE('',#18665,4.8,0.785398163397449);
#1030=CONICAL_SURFACE('',#18670,2.8,0.785398163397453);
#1031=CONICAL_SURFACE('',#18674,9.56757295257596,1.20534297321654);
#1032=CONICAL_SURFACE('',#18679,10.3,0.950546840812076);
#1033=CONICAL_SURFACE('',#18681,7.8,1.460139105621);
#1034=CONICAL_SURFACE('',#18709,5.9,0.785398163397449);
#1035=CONICAL_SURFACE('',#18721,5.9,0.785398163397449);
#1036=CONICAL_SURFACE('',#18723,3.155,0.785398163397449);
#1037=CONICAL_SURFACE('',#18730,3.155,0.785398163397448);
#1038=CONICAL_SURFACE('',#18734,4.75273145074145,1.30617281831714);
#1039=CONICAL_SURFACE('',#18741,5.41175134594813,1.04154930983939);
#1040=CONICAL_SURFACE('',#18742,5.41175134594813,1.04154930983939);
#1041=CONICAL_SURFACE('',#18743,5.41175134594813,1.04154930983939);
#1042=CONICAL_SURFACE('',#18744,5.41175134594813,1.04154930983939);
#1043=CONICAL_SURFACE('',#18745,5.41175134594813,1.04154930983939);
#1044=CONICAL_SURFACE('',#18746,5.41175134594813,1.04154930983939);
#1045=CONICAL_SURFACE('',#18762,5.41175134594813,1.04154930983939);
#1046=CONICAL_SURFACE('',#18802,2.25,0.785398163397448);
#1047=CONICAL_SURFACE('',#18805,2.35,0.785398163397447);
#1048=CONICAL_SURFACE('',#19000,2.3,0.785398163397448);
#1049=CONICAL_SURFACE('',#19005,4.75,0.785398163397448);
#1050=CONICAL_SURFACE('',#19006,4.7,0.785398163397447);
#1051=(
BOUNDED_CURVE()
B_SPLINE_CURVE(2,(#23805,#23806,#23807),.UNSPECIFIED.,.F.,.F.)
B_SPLINE_CURVE_WITH_KNOTS((3,3),(0.207879657438984,0.217458646013456),
 .UNSPECIFIED.)
CURVE()
GEOMETRIC_REPRESENTATION_ITEM()
RATIONAL_B_SPLINE_CURVE((1.00012625079627,1.0001251588785,1.00012369825994))
REPRESENTATION_ITEM('')
);
#1052=(
BOUNDED_CURVE()
B_SPLINE_CURVE(2,(#23889,#23890,#23891),.UNSPECIFIED.,.F.,.F.)
B_SPLINE_CURVE_WITH_KNOTS((3,3),(0.141563780335619,0.151142768910042),
 .UNSPECIFIED.)
CURVE()
GEOMETRIC_REPRESENTATION_ITEM()
RATIONAL_B_SPLINE_CURVE((1.00012369825443,1.00012515887293,1.00012625079065))
REPRESENTATION_ITEM('')
);
#1053=(
BOUNDED_CURVE()
B_SPLINE_CURVE(2,(#23997,#23998,#23999),.UNSPECIFIED.,.F.,.F.)
B_SPLINE_CURVE_WITH_KNOTS((3,3),(0.014211217125653,0.110567648737549),
 .UNSPECIFIED.)
CURVE()
GEOMETRIC_REPRESENTATION_ITEM()
RATIONAL_B_SPLINE_CURVE((1.00000961767885,1.00003742651076,1.00000019074343))
REPRESENTATION_ITEM('')
);
#1054=(
BOUNDED_CURVE()
B_SPLINE_CURVE(2,(#24024,#24025,#24026),.UNSPECIFIED.,.F.,.F.)
B_SPLINE_CURVE_WITH_KNOTS((3,3),(0.000246247416175969,0.0445514940289779),
 .UNSPECIFIED.)
CURVE()
GEOMETRIC_REPRESENTATION_ITEM()
RATIONAL_B_SPLINE_CURVE((1.00000019074342,1.00001731196463,1.00002068136762))
REPRESENTATION_ITEM('')
);
#1055=(
BOUNDED_CURVE()
B_SPLINE_CURVE(2,(#24030,#24031,#24032),.UNSPECIFIED.,.F.,.F.)
B_SPLINE_CURVE_WITH_KNOTS((3,3),(0.0662613029802821,0.11056581047863),
 .UNSPECIFIED.)
CURVE()
GEOMETRIC_REPRESENTATION_ITEM()
RATIONAL_B_SPLINE_CURVE((1.00002056800856,1.00001716071035,1.00000000159957))
REPRESENTATION_ITEM('')
);
#1056=(
BOUNDED_CURVE()
B_SPLINE_CURVE(2,(#24039,#24040,#24041),.UNSPECIFIED.,.F.,.F.)
B_SPLINE_CURVE_WITH_KNOTS((3,3),(7.8655962319518E-6,0.0612396373727806),
 .UNSPECIFIED.)
CURVE()
GEOMETRIC_REPRESENTATION_ITEM()
RATIONAL_B_SPLINE_CURVE((1.0000191574532,1.07458139657232,1.05821963517917))
REPRESENTATION_ITEM('')
);
#1057=(
BOUNDED_CURVE()
B_SPLINE_CURVE(2,(#24061,#24062,#24063),.UNSPECIFIED.,.F.,.F.)
B_SPLINE_CURVE_WITH_KNOTS((3,3),(0.000246247416178877,0.0966026790274259),
 .UNSPECIFIED.)
CURVE()
GEOMETRIC_REPRESENTATION_ITEM()
RATIONAL_B_SPLINE_CURVE((1.00000019074342,1.00003742650866,1.00000961767831))
REPRESENTATION_ITEM('')
);
#1058=(
BOUNDED_CURVE()
B_SPLINE_CURVE(2,(#24082,#24083,#24084),.UNSPECIFIED.,.F.,.F.)
B_SPLINE_CURVE_WITH_KNOTS((3,3),(0.0660091927117484,0.110314456526714),
 .UNSPECIFIED.)
CURVE()
GEOMETRIC_REPRESENTATION_ITEM()
RATIONAL_B_SPLINE_CURVE((1.00002048940956,1.0000171214116,1.00000000159591))
REPRESENTATION_ITEM('')
);
#1059=(
BOUNDED_CURVE()
B_SPLINE_CURVE(2,(#24091,#24092,#24093),.UNSPECIFIED.,.F.,.F.)
B_SPLINE_CURVE_WITH_KNOTS((3,3),(7.86559624534418E-6,0.0612396373727898),
 .UNSPECIFIED.)
CURVE()
GEOMETRIC_REPRESENTATION_ITEM()
RATIONAL_B_SPLINE_CURVE((1.00001915745323,1.07458139657225,1.05821963517912))
REPRESENTATION_ITEM('')
);
#1060=(
BOUNDED_CURVE()
B_SPLINE_CURVE(2,(#24098,#24099,#24100),.UNSPECIFIED.,.F.,.F.)
B_SPLINE_CURVE_WITH_KNOTS((3,3),(0.039202339545078,0.100434111321632),
 .UNSPECIFIED.)
CURVE()
GEOMETRIC_REPRESENTATION_ITEM()
RATIONAL_B_SPLINE_CURVE((1.05821963517908,1.0745813965722,1.00001915745321))
REPRESENTATION_ITEM('')
);
#1061=(
BOUNDED_CURVE()
B_SPLINE_CURVE(2,(#24123,#24124,#24125),.UNSPECIFIED.,.F.,.F.)
B_SPLINE_CURVE_WITH_KNOTS((3,3),(2.06502885214965E-6,0.0443073288438628),
 .UNSPECIFIED.)
CURVE()
GEOMETRIC_REPRESENTATION_ITEM()
RATIONAL_B_SPLINE_CURVE((1.00000000159591,1.00001712140826,1.00002048940556))
REPRESENTATION_ITEM('')
);
#1062=(
BOUNDED_CURVE()
B_SPLINE_CURVE(2,(#24127,#24128,#24129),.UNSPECIFIED.,.F.,.F.)
B_SPLINE_CURVE_WITH_KNOTS((3,3),(0.0392023395450862,0.100434111321651),
 .UNSPECIFIED.)
CURVE()
GEOMETRIC_REPRESENTATION_ITEM()
RATIONAL_B_SPLINE_CURVE((1.0582196351792,1.07458139657236,1.00001915745321))
REPRESENTATION_ITEM('')
);
#1063=(
BOUNDED_CURVE()
B_SPLINE_CURVE(2,(#24144,#24145,#24146),.UNSPECIFIED.,.F.,.F.)
B_SPLINE_CURVE_WITH_KNOTS((3,3),(0.0660091927116512,0.110314456526713),
 .UNSPECIFIED.)
CURVE()
GEOMETRIC_REPRESENTATION_ITEM()
RATIONAL_B_SPLINE_CURVE((1.00002048940626,1.00001712140884,1.00000000159591))
REPRESENTATION_ITEM('')
);
#1064=(
BOUNDED_CURVE()
B_SPLINE_CURVE(2,(#24153,#24154,#24155),.UNSPECIFIED.,.F.,.F.)
B_SPLINE_CURVE_WITH_KNOTS((3,3),(7.86559624825463E-6,0.0612396373727913),
 .UNSPECIFIED.)
CURVE()
GEOMETRIC_REPRESENTATION_ITEM()
RATIONAL_B_SPLINE_CURVE((1.00001915745324,1.07458139657224,1.0582196351791))
REPRESENTATION_ITEM('')
);
#1065=(
BOUNDED_CURVE()
B_SPLINE_CURVE(2,(#24160,#24161,#24162),.UNSPECIFIED.,.F.,.F.)
B_SPLINE_CURVE_WITH_KNOTS((3,3),(0.0392023395450792,0.100434111321637),
 .UNSPECIFIED.)
CURVE()
GEOMETRIC_REPRESENTATION_ITEM()
RATIONAL_B_SPLINE_CURVE((1.05821963517906,1.07458139657217,1.00001915745318))
REPRESENTATION_ITEM('')
);
#1066=(
BOUNDED_CURVE()
B_SPLINE_CURVE(2,(#24183,#24184,#24185),.UNSPECIFIED.,.F.,.F.)
B_SPLINE_CURVE_WITH_KNOTS((3,3),(2.06502885258463E-6,0.0443073288438806),
 .UNSPECIFIED.)
CURVE()
GEOMETRIC_REPRESENTATION_ITEM()
RATIONAL_B_SPLINE_CURVE((1.00000000159591,1.00001712141144,1.00002048940937))
REPRESENTATION_ITEM('')
);
#1067=(
BOUNDED_CURVE()
B_SPLINE_CURVE(2,(#24191,#24192,#24193),.UNSPECIFIED.,.F.,.F.)
B_SPLINE_CURVE_WITH_KNOTS((3,3),(2.06499351918632E-6,0.0443065724919368),
 .UNSPECIFIED.)
CURVE()
GEOMETRIC_REPRESENTATION_ITEM()
RATIONAL_B_SPLINE_CURVE((1.00000000159957,1.00001716071329,1.00002056801208))
REPRESENTATION_ITEM('')
);
#1068=(
BOUNDED_CURVE()
B_SPLINE_CURVE(2,(#24201,#24202,#24203),.UNSPECIFIED.,.F.,.F.)
B_SPLINE_CURVE_WITH_KNOTS((3,3),(0.000246247280288311,0.0966026259860039),
 .UNSPECIFIED.)
CURVE()
GEOMETRIC_REPRESENTATION_ITEM()
RATIONAL_B_SPLINE_CURVE((1.00000019075751,1.00003742928082,1.00000962320604))
REPRESENTATION_ITEM('')
);
#1069=(
BOUNDED_CURVE()
B_SPLINE_CURVE(2,(#24238,#24239,#24240),.UNSPECIFIED.,.F.,.F.)
B_SPLINE_CURVE_WITH_KNOTS((3,3),(0.0662687847811497,0.110573269834419),
 .UNSPECIFIED.)
CURVE()
GEOMETRIC_REPRESENTATION_ITEM()
RATIONAL_B_SPLINE_CURVE((1.00002057035038,1.00001716188432,1.00000000159968))
REPRESENTATION_ITEM('')
);
#1070=(
BOUNDED_CURVE()
B_SPLINE_CURVE(2,(#24247,#24248,#24249),.UNSPECIFIED.,.F.,.F.)
B_SPLINE_CURVE_WITH_KNOTS((3,3),(7.86559623378178E-6,0.0612396373727884),
 .UNSPECIFIED.)
CURVE()
GEOMETRIC_REPRESENTATION_ITEM()
RATIONAL_B_SPLINE_CURVE((1.00001915745321,1.07458139657226,1.05821963517913))
REPRESENTATION_ITEM('')
);
#1071=(
BOUNDED_CURVE()
B_SPLINE_CURVE(2,(#24280,#24281,#24282),.UNSPECIFIED.,.F.,.F.)
B_SPLINE_CURVE_WITH_KNOTS((3,3),(2.06502884978116E-6,0.0443073288439222),
 .UNSPECIFIED.)
CURVE()
GEOMETRIC_REPRESENTATION_ITEM()
RATIONAL_B_SPLINE_CURVE((1.00000000159591,1.0000171214099,1.00002048940752))
REPRESENTATION_ITEM('')
);
#1072=(
BOUNDED_CURVE()
B_SPLINE_CURVE(2,(#24284,#24285,#24286),.UNSPECIFIED.,.F.,.F.)
B_SPLINE_CURVE_WITH_KNOTS((3,3),(0.0392023395450863,0.100434111321653),
 .UNSPECIFIED.)
CURVE()
GEOMETRIC_REPRESENTATION_ITEM()
RATIONAL_B_SPLINE_CURVE((1.0582196351792,1.07458139657235,1.00001915745318))
REPRESENTATION_ITEM('')
);
#1073=(
BOUNDED_CURVE()
B_SPLINE_CURVE(2,(#24292,#24293,#24294),.UNSPECIFIED.,.F.,.F.)
B_SPLINE_CURVE_WITH_KNOTS((3,3),(0.0660091927117005,0.110314456526681),
 .UNSPECIFIED.)
CURVE()
GEOMETRIC_REPRESENTATION_ITEM()
RATIONAL_B_SPLINE_CURVE((1.00002048940979,1.0000171214118,1.00000000159591))
REPRESENTATION_ITEM('')
);
#1074=(
BOUNDED_CURVE()
B_SPLINE_CURVE(2,(#24315,#24316,#24317),.UNSPECIFIED.,.F.,.F.)
B_SPLINE_CURVE_WITH_KNOTS((3,3),(7.86559623866961E-6,0.0612396373727917),
 .UNSPECIFIED.)
CURVE()
GEOMETRIC_REPRESENTATION_ITEM()
RATIONAL_B_SPLINE_CURVE((1.00001915745322,1.07458139657226,1.05821963517913))
REPRESENTATION_ITEM('')
);
#1075=(
BOUNDED_CURVE()
B_SPLINE_CURVE(2,(#24325,#24326,#24327),.UNSPECIFIED.,.F.,.F.)
B_SPLINE_CURVE_WITH_KNOTS((3,3),(2.06502884929736E-6,0.0443073288439272),
 .UNSPECIFIED.)
CURVE()
GEOMETRIC_REPRESENTATION_ITEM()
RATIONAL_B_SPLINE_CURVE((1.00000000159591,1.0000171214054,1.00002048940214))
REPRESENTATION_ITEM('')
);
#1076=(
BOUNDED_CURVE()
B_SPLINE_CURVE(2,(#24329,#24330,#24331),.UNSPECIFIED.,.F.,.F.)
B_SPLINE_CURVE_WITH_KNOTS((3,3),(0.0392023395450894,0.100434111321656),
 .UNSPECIFIED.)
CURVE()
GEOMETRIC_REPRESENTATION_ITEM()
RATIONAL_B_SPLINE_CURVE((1.05821963517919,1.07458139657234,1.00001915745318))
REPRESENTATION_ITEM('')
);
#1077=(
BOUNDED_CURVE()
B_SPLINE_CURVE(2,(#24337,#24338,#24339),.UNSPECIFIED.,.F.,.F.)
B_SPLINE_CURVE_WITH_KNOTS((3,3),(0.066009192711667,0.110314456526716),
 .UNSPECIFIED.)
CURVE()
GEOMETRIC_REPRESENTATION_ITEM()
RATIONAL_B_SPLINE_CURVE((1.00002048940695,1.00001712140941,1.00000000159591))
REPRESENTATION_ITEM('')
);
#1078=(
BOUNDED_CURVE()
B_SPLINE_CURVE(2,(#24360,#24361,#24362),.UNSPECIFIED.,.F.,.F.)
B_SPLINE_CURVE_WITH_KNOTS((3,3),(7.86559624154099E-6,0.061239637372789),
 .UNSPECIFIED.)
CURVE()
GEOMETRIC_REPRESENTATION_ITEM()
RATIONAL_B_SPLINE_CURVE((1.00001915745323,1.07458139657237,1.05821963517921))
REPRESENTATION_ITEM('')
);
#1079=(
BOUNDED_CURVE()
B_SPLINE_CURVE(2,(#24370,#24371,#24372),.UNSPECIFIED.,.F.,.F.)
B_SPLINE_CURVE_WITH_KNOTS((3,3),(2.06502884995711E-6,0.0443073288438823),
 .UNSPECIFIED.)
CURVE()
GEOMETRIC_REPRESENTATION_ITEM()
RATIONAL_B_SPLINE_CURVE((1.00000000159591,1.00001712141098,1.00002048940882))
REPRESENTATION_ITEM('')
);
#1080=(
BOUNDED_CURVE()
B_SPLINE_CURVE(2,(#24374,#24375,#24376),.UNSPECIFIED.,.F.,.F.)
B_SPLINE_CURVE_WITH_KNOTS((3,3),(0.0392023395450777,0.100434111321635),
 .UNSPECIFIED.)
CURVE()
GEOMETRIC_REPRESENTATION_ITEM()
RATIONAL_B_SPLINE_CURVE((1.05821963517909,1.07458139657222,1.0000191574532))
REPRESENTATION_ITEM('')
);
#1081=(
BOUNDED_CURVE()
B_SPLINE_CURVE(2,(#24382,#24383,#24384),.UNSPECIFIED.,.F.,.F.)
B_SPLINE_CURVE_WITH_KNOTS((3,3),(0.066009192711704,0.110314456526683),
 .UNSPECIFIED.)
CURVE()
GEOMETRIC_REPRESENTATION_ITEM()
RATIONAL_B_SPLINE_CURVE((1.0000204894117,1.00001712141339,1.00000000159591))
REPRESENTATION_ITEM('')
);
#1082=(
BOUNDED_CURVE()
B_SPLINE_CURVE(2,(#24405,#24406,#24407),.UNSPECIFIED.,.F.,.F.)
B_SPLINE_CURVE_WITH_KNOTS((3,3),(7.86559624762531E-6,0.0612396373728004),
 .UNSPECIFIED.)
CURVE()
GEOMETRIC_REPRESENTATION_ITEM()
RATIONAL_B_SPLINE_CURVE((1.00001915745324,1.07458139657236,1.0582196351792))
REPRESENTATION_ITEM('')
);
#1083=(
BOUNDED_CURVE()
B_SPLINE_CURVE(2,(#24415,#24416,#24417),.UNSPECIFIED.,.F.,.F.)
B_SPLINE_CURVE_WITH_KNOTS((3,3),(2.06502884960702E-6,0.0443073288440253),
 .UNSPECIFIED.)
CURVE()
GEOMETRIC_REPRESENTATION_ITEM()
RATIONAL_B_SPLINE_CURVE((1.00000000159591,1.00001712140153,1.00002048939751))
REPRESENTATION_ITEM('')
);
#1084=(
BOUNDED_CURVE()
B_SPLINE_CURVE(2,(#24419,#24420,#24421),.UNSPECIFIED.,.F.,.F.)
B_SPLINE_CURVE_WITH_KNOTS((3,3),(0.0392023395450754,0.100434111321632),
 .UNSPECIFIED.)
CURVE()
GEOMETRIC_REPRESENTATION_ITEM()
RATIONAL_B_SPLINE_CURVE((1.05821963517911,1.07458139657224,1.00001915745321))
REPRESENTATION_ITEM('')
);
#1085=(
BOUNDED_CURVE()
B_SPLINE_CURVE(2,(#24427,#24428,#24429),.UNSPECIFIED.,.F.,.F.)
B_SPLINE_CURVE_WITH_KNOTS((3,3),(0.066009192711622,0.110314456526713),
 .UNSPECIFIED.)
CURVE()
GEOMETRIC_REPRESENTATION_ITEM()
RATIONAL_B_SPLINE_CURVE((1.00002048940407,1.00001712140701,1.00000000159591))
REPRESENTATION_ITEM('')
);
#1086=(
BOUNDED_CURVE()
B_SPLINE_CURVE(2,(#24450,#24451,#24452),.UNSPECIFIED.,.F.,.F.)
B_SPLINE_CURVE_WITH_KNOTS((3,3),(7.86559623771071E-6,0.0612396373727852),
 .UNSPECIFIED.)
CURVE()
GEOMETRIC_REPRESENTATION_ITEM()
RATIONAL_B_SPLINE_CURVE((1.00001915745322,1.07458139657238,1.05821963517921))
REPRESENTATION_ITEM('')
);
#1087=(
BOUNDED_CURVE()
B_SPLINE_CURVE(2,(#24460,#24461,#24462),.UNSPECIFIED.,.F.,.F.)
B_SPLINE_CURVE_WITH_KNOTS((3,3),(2.06502884816085E-6,0.0443073288439097),
 .UNSPECIFIED.)
CURVE()
GEOMETRIC_REPRESENTATION_ITEM()
RATIONAL_B_SPLINE_CURVE((1.00000000159591,1.00001712140925,1.00002048940675))
REPRESENTATION_ITEM('')
);
#1088=(
BOUNDED_CURVE()
B_SPLINE_CURVE(2,(#24464,#24465,#24466),.UNSPECIFIED.,.F.,.F.)
B_SPLINE_CURVE_WITH_KNOTS((3,3),(0.0392023395450782,0.100434111321637),
 .UNSPECIFIED.)
CURVE()
GEOMETRIC_REPRESENTATION_ITEM()
RATIONAL_B_SPLINE_CURVE((1.05821963517907,1.07458139657219,1.00001915745318))
REPRESENTATION_ITEM('')
);
#1089=(
BOUNDED_CURVE()
B_SPLINE_CURVE(2,(#24472,#24473,#24474),.UNSPECIFIED.,.F.,.F.)
B_SPLINE_CURVE_WITH_KNOTS((3,3),(0.0660091927116034,0.110314456526687),
 .UNSPECIFIED.)
CURVE()
GEOMETRIC_REPRESENTATION_ITEM()
RATIONAL_B_SPLINE_CURVE((1.00002048940631,1.00001712140889,1.00000000159591))
REPRESENTATION_ITEM('')
);
#1090=(
BOUNDED_CURVE()
B_SPLINE_CURVE(2,(#24495,#24496,#24497),.UNSPECIFIED.,.F.,.F.)
B_SPLINE_CURVE_WITH_KNOTS((3,3),(7.86559625577519E-6,0.061239637372806),
 .UNSPECIFIED.)
CURVE()
GEOMETRIC_REPRESENTATION_ITEM()
RATIONAL_B_SPLINE_CURVE((1.00001915745326,1.07458139657232,1.05821963517917))
REPRESENTATION_ITEM('')
);
#1091=(
BOUNDED_CURVE()
B_SPLINE_CURVE(2,(#24505,#24506,#24507),.UNSPECIFIED.,.F.,.F.)
B_SPLINE_CURVE_WITH_KNOTS((3,3),(2.06502884983613E-6,0.0443073288439088),
 .UNSPECIFIED.)
CURVE()
GEOMETRIC_REPRESENTATION_ITEM()
RATIONAL_B_SPLINE_CURVE((1.00000000159591,1.00001712140953,1.00002048940709))
REPRESENTATION_ITEM('')
);
#1092=(
BOUNDED_CURVE()
B_SPLINE_CURVE(2,(#24509,#24510,#24511),.UNSPECIFIED.,.F.,.F.)
B_SPLINE_CURVE_WITH_KNOTS((3,3),(0.0392023395450886,0.10043411132165),
 .UNSPECIFIED.)
CURVE()
GEOMETRIC_REPRESENTATION_ITEM()
RATIONAL_B_SPLINE_CURVE((1.05821963517901,1.07458139657211,1.00001915745323))
REPRESENTATION_ITEM('')
);
#1093=(
BOUNDED_CURVE()
B_SPLINE_CURVE(2,(#24517,#24518,#24519),.UNSPECIFIED.,.F.,.F.)
B_SPLINE_CURVE_WITH_KNOTS((3,3),(0.0660091927116451,0.110314456526683),
 .UNSPECIFIED.)
CURVE()
GEOMETRIC_REPRESENTATION_ITEM()
RATIONAL_B_SPLINE_CURVE((1.00002048940605,1.00001712140867,1.00000000159591))
REPRESENTATION_ITEM('')
);
#1094=(
BOUNDED_CURVE()
B_SPLINE_CURVE(2,(#24540,#24541,#24542),.UNSPECIFIED.,.F.,.F.)
B_SPLINE_CURVE_WITH_KNOTS((3,3),(7.86559624689154E-6,0.061239637372801),
 .UNSPECIFIED.)
CURVE()
GEOMETRIC_REPRESENTATION_ITEM()
RATIONAL_B_SPLINE_CURVE((1.00001915745324,1.07458139657241,1.05821963517924))
REPRESENTATION_ITEM('')
);
#1095=(
BOUNDED_CURVE()
B_SPLINE_CURVE(2,(#24550,#24551,#24552),.UNSPECIFIED.,.F.,.F.)
B_SPLINE_CURVE_WITH_KNOTS((3,3),(2.0650288490547E-6,0.0443073288439657),
 .UNSPECIFIED.)
CURVE()
GEOMETRIC_REPRESENTATION_ITEM()
RATIONAL_B_SPLINE_CURVE((1.00000000159591,1.00001712141033,1.00002048940803))
REPRESENTATION_ITEM('')
);
#1096=(
BOUNDED_CURVE()
B_SPLINE_CURVE(2,(#24554,#24555,#24556),.UNSPECIFIED.,.F.,.F.)
B_SPLINE_CURVE_WITH_KNOTS((3,3),(0.0392023395450856,0.100434111321651),
 .UNSPECIFIED.)
CURVE()
GEOMETRIC_REPRESENTATION_ITEM()
RATIONAL_B_SPLINE_CURVE((1.0582196351791,1.07458139657223,1.0000191574532))
REPRESENTATION_ITEM('')
);
#1097=(
BOUNDED_CURVE()
B_SPLINE_CURVE(2,(#24562,#24563,#24564),.UNSPECIFIED.,.F.,.F.)
B_SPLINE_CURVE_WITH_KNOTS((3,3),(0.0660091927115862,0.110314456526683),
 .UNSPECIFIED.)
CURVE()
GEOMETRIC_REPRESENTATION_ITEM()
RATIONAL_B_SPLINE_CURVE((1.00002048940501,1.00001712140779,1.00000000159591))
REPRESENTATION_ITEM('')
);
#1098=(
BOUNDED_CURVE()
B_SPLINE_CURVE(2,(#24585,#24586,#24587),.UNSPECIFIED.,.F.,.F.)
B_SPLINE_CURVE_WITH_KNOTS((3,3),(7.86559623861992E-6,0.0612396373727923),
 .UNSPECIFIED.)
CURVE()
GEOMETRIC_REPRESENTATION_ITEM()
RATIONAL_B_SPLINE_CURVE((1.00001915745322,1.07458139657228,1.05821963517915))
REPRESENTATION_ITEM('')
);
#1099=(
BOUNDED_CURVE()
B_SPLINE_CURVE(2,(#24595,#24596,#24597),.UNSPECIFIED.,.F.,.F.)
B_SPLINE_CURVE_WITH_KNOTS((3,3),(2.06502884791252E-6,0.0443073288439309),
 .UNSPECIFIED.)
CURVE()
GEOMETRIC_REPRESENTATION_ITEM()
RATIONAL_B_SPLINE_CURVE((1.00000000159591,1.00001712140764,1.00002048940482))
REPRESENTATION_ITEM('')
);
#1100=(
BOUNDED_CURVE()
B_SPLINE_CURVE(2,(#24599,#24600,#24601),.UNSPECIFIED.,.F.,.F.)
B_SPLINE_CURVE_WITH_KNOTS((3,3),(0.0392023395450768,0.100434111321634),
 .UNSPECIFIED.)
CURVE()
GEOMETRIC_REPRESENTATION_ITEM()
RATIONAL_B_SPLINE_CURVE((1.05821963517911,1.07458139657224,1.00001915745319))
REPRESENTATION_ITEM('')
);
#1101=(
BOUNDED_CURVE()
B_SPLINE_CURVE(2,(#24607,#24608,#24609),.UNSPECIFIED.,.F.,.F.)
B_SPLINE_CURVE_WITH_KNOTS((3,3),(0.0660091927116233,0.11031445652668),
 .UNSPECIFIED.)
CURVE()
GEOMETRIC_REPRESENTATION_ITEM()
RATIONAL_B_SPLINE_CURVE((1.00002048941031,1.00001712141222,1.00000000159591))
REPRESENTATION_ITEM('')
);
#1102=(
BOUNDED_CURVE()
B_SPLINE_CURVE(2,(#24630,#24631,#24632),.UNSPECIFIED.,.F.,.F.)
B_SPLINE_CURVE_WITH_KNOTS((3,3),(7.8735648790627E-6,0.0613120861126728),
 .UNSPECIFIED.)
CURVE()
GEOMETRIC_REPRESENTATION_ITEM()
RATIONAL_B_SPLINE_CURVE((1.00001920106114,1.0747638688358,1.05857900734984))
REPRESENTATION_ITEM('')
);
#1103=(
BOUNDED_CURVE()
B_SPLINE_CURVE(2,(#24637,#24638,#24639),.UNSPECIFIED.,.F.,.F.)
B_SPLINE_CURVE_WITH_KNOTS((3,3),(0.0392028994779419,0.100212511691547),
 .UNSPECIFIED.)
CURVE()
GEOMETRIC_REPRESENTATION_ITEM()
RATIONAL_B_SPLINE_CURVE((1.06060654550647,1.0784249750017,1.00491903156505))
REPRESENTATION_ITEM('')
);
#1104=(
BOUNDED_CURVE()
B_SPLINE_CURVE(2,(#24658,#24659,#24660),.UNSPECIFIED.,.F.,.F.)
B_SPLINE_CURVE_WITH_KNOTS((3,3),(2.36858664140126,2.48027053188039),
 .UNSPECIFIED.)
CURVE()
GEOMETRIC_REPRESENTATION_ITEM()
RATIONAL_B_SPLINE_CURVE((1.00156925623442,1.0009208220165,1.00020774873445))
REPRESENTATION_ITEM('')
);
#1105=(
BOUNDED_CURVE()
B_SPLINE_CURVE(2,(#24994,#24995,#24996),.UNSPECIFIED.,.F.,.F.)
B_SPLINE_CURVE_WITH_KNOTS((3,3),(0.066268784781115,0.11057326983442),
 .UNSPECIFIED.)
CURVE()
GEOMETRIC_REPRESENTATION_ITEM()
RATIONAL_B_SPLINE_CURVE((1.00002057034838,1.00001716188265,1.00000000159968))
REPRESENTATION_ITEM('')
);
#1106=(
BOUNDED_CURVE()
B_SPLINE_CURVE(2,(#25003,#25004,#25005),.UNSPECIFIED.,.F.,.F.)
B_SPLINE_CURVE_WITH_KNOTS((3,3),(7.86559624521441E-6,0.0612396373727986),
 .UNSPECIFIED.)
CURVE()
GEOMETRIC_REPRESENTATION_ITEM()
RATIONAL_B_SPLINE_CURVE((1.00001915745323,1.07458139657223,1.05821963517911))
REPRESENTATION_ITEM('')
);
#1107=(
BOUNDED_CURVE()
B_SPLINE_CURVE(2,(#25010,#25011,#25012),.UNSPECIFIED.,.F.,.F.)
B_SPLINE_CURVE_WITH_KNOTS((3,3),(0.039202339545088,0.100434111321661),
 .UNSPECIFIED.)
CURVE()
GEOMETRIC_REPRESENTATION_ITEM()
RATIONAL_B_SPLINE_CURVE((1.05821963517928,1.07458139657247,1.00001915745322))
REPRESENTATION_ITEM('')
);
#1108=(
BOUNDED_CURVE()
B_SPLINE_CURVE(2,(#25030,#25031,#25032),.UNSPECIFIED.,.F.,.F.)
B_SPLINE_CURVE_WITH_KNOTS((3,3),(2.06502885058066E-6,0.0443073288438408),
 .UNSPECIFIED.)
CURVE()
GEOMETRIC_REPRESENTATION_ITEM()
RATIONAL_B_SPLINE_CURVE((1.00000000159591,1.00001712141098,1.00002048940882))
REPRESENTATION_ITEM('')
);
#1109=(
BOUNDED_CURVE()
B_SPLINE_CURVE(2,(#25036,#25037,#25038),.UNSPECIFIED.,.F.,.F.)
B_SPLINE_CURVE_WITH_KNOTS((3,3),(0.066009192711637,0.110314456526716),
 .UNSPECIFIED.)
CURVE()
GEOMETRIC_REPRESENTATION_ITEM()
RATIONAL_B_SPLINE_CURVE((1.00002048940915,1.00001712141126,1.00000000159591))
REPRESENTATION_ITEM('')
);
#1110=(
BOUNDED_CURVE()
B_SPLINE_CURVE(2,(#25045,#25046,#25047),.UNSPECIFIED.,.F.,.F.)
B_SPLINE_CURVE_WITH_KNOTS((3,3),(7.86559623619297E-6,0.06123963737278),
 .UNSPECIFIED.)
CURVE()
GEOMETRIC_REPRESENTATION_ITEM()
RATIONAL_B_SPLINE_CURVE((1.00001915745321,1.0745813965721,1.058219635179))
REPRESENTATION_ITEM('')
);
#1111=(
BOUNDED_CURVE()
B_SPLINE_CURVE(2,(#25052,#25053,#25054),.UNSPECIFIED.,.F.,.F.)
B_SPLINE_CURVE_WITH_KNOTS((3,3),(0.039202339545078,0.100434111321636),
 .UNSPECIFIED.)
CURVE()
GEOMETRIC_REPRESENTATION_ITEM()
RATIONAL_B_SPLINE_CURVE((1.05821963517909,1.07458139657222,1.0000191574532))
REPRESENTATION_ITEM('')
);
#1112=(
BOUNDED_CURVE()
B_SPLINE_CURVE(2,(#25072,#25073,#25074),.UNSPECIFIED.,.F.,.F.)
B_SPLINE_CURVE_WITH_KNOTS((3,3),(2.06502885091957E-6,0.0443073288439418),
 .UNSPECIFIED.)
CURVE()
GEOMETRIC_REPRESENTATION_ITEM()
RATIONAL_B_SPLINE_CURVE((1.00000000159591,1.00001712141366,1.00002048941202))
REPRESENTATION_ITEM('')
);
#1113=(
BOUNDED_CURVE()
B_SPLINE_CURVE(2,(#25078,#25079,#25080),.UNSPECIFIED.,.F.,.F.)
B_SPLINE_CURVE_WITH_KNOTS((3,3),(0.066009192711676,0.110314456526716),
 .UNSPECIFIED.)
CURVE()
GEOMETRIC_REPRESENTATION_ITEM()
RATIONAL_B_SPLINE_CURVE((1.00002048941196,1.0000171214136,1.00000000159591))
REPRESENTATION_ITEM('')
);
#1114=(
BOUNDED_CURVE()
B_SPLINE_CURVE(2,(#25087,#25088,#25089),.UNSPECIFIED.,.F.,.F.)
B_SPLINE_CURVE_WITH_KNOTS((3,3),(7.86559624634883E-6,0.0612396373727915),
 .UNSPECIFIED.)
CURVE()
GEOMETRIC_REPRESENTATION_ITEM()
RATIONAL_B_SPLINE_CURVE((1.00001915745324,1.07458139657221,1.05821963517909))
REPRESENTATION_ITEM('')
);
#1115=(
BOUNDED_CURVE()
B_SPLINE_CURVE(2,(#25094,#25095,#25096),.UNSPECIFIED.,.F.,.F.)
B_SPLINE_CURVE_WITH_KNOTS((3,3),(0.0392023395450874,0.100434111321651),
 .UNSPECIFIED.)
CURVE()
GEOMETRIC_REPRESENTATION_ITEM()
RATIONAL_B_SPLINE_CURVE((1.05821963517914,1.07458139657228,1.00001915745321))
REPRESENTATION_ITEM('')
);
#1116=(
BOUNDED_CURVE()
B_SPLINE_CURVE(2,(#25111,#25112,#25113),.UNSPECIFIED.,.F.,.F.)
B_SPLINE_CURVE_WITH_KNOTS((3,3),(0.0142112171257214,0.110567648737575),
 .UNSPECIFIED.)
CURVE()
GEOMETRIC_REPRESENTATION_ITEM()
RATIONAL_B_SPLINE_CURVE((1.00000961767768,1.0000374265062,1.0000001907434))
REPRESENTATION_ITEM('')
);
#1117=(
BOUNDED_CURVE()
B_SPLINE_CURVE(2,(#25124,#25125,#25126),.UNSPECIFIED.,.F.,.F.)
B_SPLINE_CURVE_WITH_KNOTS((3,3),(0.000246247416174898,0.0445514940289623),
 .UNSPECIFIED.)
CURVE()
GEOMETRIC_REPRESENTATION_ITEM()
RATIONAL_B_SPLINE_CURVE((1.00000019074344,1.00001731196687,1.00002068137031))
REPRESENTATION_ITEM('')
);
#1118=(
BOUNDED_CURVE()
B_SPLINE_CURVE(2,(#25136,#25137,#25138),.UNSPECIFIED.,.F.,.F.)
B_SPLINE_CURVE_WITH_KNOTS((3,3),(0.000246247416180695,0.0966026790274006),
 .UNSPECIFIED.)
CURVE()
GEOMETRIC_REPRESENTATION_ITEM()
RATIONAL_B_SPLINE_CURVE((1.00000019074341,1.00003742650782,1.00000961767809))
REPRESENTATION_ITEM('')
);
#1119=(
BOUNDED_CURVE()
B_SPLINE_CURVE(2,(#25144,#25145,#25146),.UNSPECIFIED.,.F.,.F.)
B_SPLINE_CURVE_WITH_KNOTS((3,3),(0.0662624021247591,0.110567648737568),
 .UNSPECIFIED.)
CURVE()
GEOMETRIC_REPRESENTATION_ITEM()
RATIONAL_B_SPLINE_CURVE((1.00002068136531,1.00001731196269,1.0000001907434))
REPRESENTATION_ITEM('')
);
#1120=(
BOUNDED_CURVE()
B_SPLINE_CURVE(2,(#25164,#25165,#25166),.UNSPECIFIED.,.F.,.F.)
B_SPLINE_CURVE_WITH_KNOTS((3,3),(7.86559624155621E-6,0.0612396373727861),
 .UNSPECIFIED.)
CURVE()
GEOMETRIC_REPRESENTATION_ITEM()
RATIONAL_B_SPLINE_CURVE((1.00001915745323,1.07458139657213,1.05821963517903))
REPRESENTATION_ITEM('')
);
#1121=(
BOUNDED_CURVE()
B_SPLINE_CURVE(2,(#25174,#25175,#25176),.UNSPECIFIED.,.F.,.F.)
B_SPLINE_CURVE_WITH_KNOTS((3,3),(2.06502885047952E-6,0.0443073288439063),
 .UNSPECIFIED.)
CURVE()
GEOMETRIC_REPRESENTATION_ITEM()
RATIONAL_B_SPLINE_CURVE((1.00000000159591,1.00001712141005,1.00002048940771))
REPRESENTATION_ITEM('')
);
#1122=(
BOUNDED_CURVE()
B_SPLINE_CURVE(2,(#25178,#25179,#25180),.UNSPECIFIED.,.F.,.F.)
B_SPLINE_CURVE_WITH_KNOTS((3,3),(0.039202339545091,0.100434111321655),
 .UNSPECIFIED.)
CURVE()
GEOMETRIC_REPRESENTATION_ITEM()
RATIONAL_B_SPLINE_CURVE((1.05821963517907,1.07458139657219,1.0000191574532))
REPRESENTATION_ITEM('')
);
#1123=(
BOUNDED_CURVE()
B_SPLINE_CURVE(2,(#25186,#25187,#25188),.UNSPECIFIED.,.F.,.F.)
B_SPLINE_CURVE_WITH_KNOTS((3,3),(0.0660091927117379,0.110314456526716),
 .UNSPECIFIED.)
CURVE()
GEOMETRIC_REPRESENTATION_ITEM()
RATIONAL_B_SPLINE_CURVE((1.00002048940992,1.0000171214119,1.00000000159591))
REPRESENTATION_ITEM('')
);
#1124=(
BOUNDED_CURVE()
B_SPLINE_CURVE(2,(#25206,#25207,#25208),.UNSPECIFIED.,.F.,.F.)
B_SPLINE_CURVE_WITH_KNOTS((3,3),(7.86559624404147E-6,0.0612396373727875),
 .UNSPECIFIED.)
CURVE()
GEOMETRIC_REPRESENTATION_ITEM()
RATIONAL_B_SPLINE_CURVE((1.00001915745323,1.07458139657229,1.05821963517915))
REPRESENTATION_ITEM('')
);
#1125=(
BOUNDED_CURVE()
B_SPLINE_CURVE(2,(#25216,#25217,#25218),.UNSPECIFIED.,.F.,.F.)
B_SPLINE_CURVE_WITH_KNOTS((3,3),(2.06502885034354E-6,0.0443073288439307),
 .UNSPECIFIED.)
CURVE()
GEOMETRIC_REPRESENTATION_ITEM()
RATIONAL_B_SPLINE_CURVE((1.00000000159591,1.00001712141048,1.00002048940822))
REPRESENTATION_ITEM('')
);
#1126=(
BOUNDED_CURVE()
B_SPLINE_CURVE(2,(#25220,#25221,#25222),.UNSPECIFIED.,.F.,.F.)
B_SPLINE_CURVE_WITH_KNOTS((3,3),(0.039202339545077,0.100434111321635),
 .UNSPECIFIED.)
CURVE()
GEOMETRIC_REPRESENTATION_ITEM()
RATIONAL_B_SPLINE_CURVE((1.05821963517913,1.07458139657227,1.00001915745318))
REPRESENTATION_ITEM('')
);
#1127=(
BOUNDED_CURVE()
B_SPLINE_CURVE(2,(#25228,#25229,#25230),.UNSPECIFIED.,.F.,.F.)
B_SPLINE_CURVE_WITH_KNOTS((3,3),(0.0660091927115155,0.110314456526713),
 .UNSPECIFIED.)
CURVE()
GEOMETRIC_REPRESENTATION_ITEM()
RATIONAL_B_SPLINE_CURVE((1.00002048939951,1.0000171214032,1.00000000159591))
REPRESENTATION_ITEM('')
);
#1128=(
BOUNDED_CURVE()
B_SPLINE_CURVE(2,(#25248,#25249,#25250),.UNSPECIFIED.,.F.,.F.)
B_SPLINE_CURVE_WITH_KNOTS((3,3),(7.8655962495386E-6,0.0612396373727939),
 .UNSPECIFIED.)
CURVE()
GEOMETRIC_REPRESENTATION_ITEM()
RATIONAL_B_SPLINE_CURVE((1.00001915745324,1.07458139657231,1.05821963517916))
REPRESENTATION_ITEM('')
);
#1129=(
BOUNDED_CURVE()
B_SPLINE_CURVE(2,(#25258,#25259,#25260),.UNSPECIFIED.,.F.,.F.)
B_SPLINE_CURVE_WITH_KNOTS((3,3),(2.06502884777574E-6,0.0443073288439337),
 .UNSPECIFIED.)
CURVE()
GEOMETRIC_REPRESENTATION_ITEM()
RATIONAL_B_SPLINE_CURVE((1.00000000159591,1.00001712140949,1.00002048940703))
REPRESENTATION_ITEM('')
);
#1130=(
BOUNDED_CURVE()
B_SPLINE_CURVE(2,(#25262,#25263,#25264),.UNSPECIFIED.,.F.,.F.)
B_SPLINE_CURVE_WITH_KNOTS((3,3),(0.0392023395450778,0.100434111321633),
 .UNSPECIFIED.)
CURVE()
GEOMETRIC_REPRESENTATION_ITEM()
RATIONAL_B_SPLINE_CURVE((1.05821963517902,1.07458139657213,1.00001915745319))
REPRESENTATION_ITEM('')
);
#1131=(
BOUNDED_CURVE()
B_SPLINE_CURVE(2,(#25270,#25271,#25272),.UNSPECIFIED.,.F.,.F.)
B_SPLINE_CURVE_WITH_KNOTS((3,3),(0.0660091927116281,0.110314456526714),
 .UNSPECIFIED.)
CURVE()
GEOMETRIC_REPRESENTATION_ITEM()
RATIONAL_B_SPLINE_CURVE((1.00002048941071,1.00001712141256,1.00000000159591))
REPRESENTATION_ITEM('')
);
#1132=(
BOUNDED_CURVE()
B_SPLINE_CURVE(2,(#25290,#25291,#25292),.UNSPECIFIED.,.F.,.F.)
B_SPLINE_CURVE_WITH_KNOTS((3,3),(7.86559623181466E-6,0.061239637372782),
 .UNSPECIFIED.)
CURVE()
GEOMETRIC_REPRESENTATION_ITEM()
RATIONAL_B_SPLINE_CURVE((1.0000191574532,1.07458139657242,1.05821963517925))
REPRESENTATION_ITEM('')
);
#1133=(
BOUNDED_CURVE()
B_SPLINE_CURVE(2,(#25300,#25301,#25302),.UNSPECIFIED.,.F.,.F.)
B_SPLINE_CURVE_WITH_KNOTS((3,3),(2.06502885033157E-6,0.0443073288437829),
 .UNSPECIFIED.)
CURVE()
GEOMETRIC_REPRESENTATION_ITEM()
RATIONAL_B_SPLINE_CURVE((1.00000000159591,1.00001712141826,1.00002048941753))
REPRESENTATION_ITEM('')
);
#1134=(
BOUNDED_CURVE()
B_SPLINE_CURVE(2,(#25304,#25305,#25306),.UNSPECIFIED.,.F.,.F.)
B_SPLINE_CURVE_WITH_KNOTS((3,3),(0.0392023395450864,0.100434111321655),
 .UNSPECIFIED.)
CURVE()
GEOMETRIC_REPRESENTATION_ITEM()
RATIONAL_B_SPLINE_CURVE((1.05821963517922,1.07458139657238,1.00001915745319))
REPRESENTATION_ITEM('')
);
#1135=(
BOUNDED_CURVE()
B_SPLINE_CURVE(2,(#25312,#25313,#25314),.UNSPECIFIED.,.F.,.F.)
B_SPLINE_CURVE_WITH_KNOTS((3,3),(0.06600919271163,0.110314456526716),
 .UNSPECIFIED.)
CURVE()
GEOMETRIC_REPRESENTATION_ITEM()
RATIONAL_B_SPLINE_CURVE((1.00002048941218,1.00001712141379,1.00000000159591))
REPRESENTATION_ITEM('')
);
#1136=(
BOUNDED_CURVE()
B_SPLINE_CURVE(2,(#25332,#25333,#25334),.UNSPECIFIED.,.F.,.F.)
B_SPLINE_CURVE_WITH_KNOTS((3,3),(7.86559623262009E-6,0.0612396373727778),
 .UNSPECIFIED.)
CURVE()
GEOMETRIC_REPRESENTATION_ITEM()
RATIONAL_B_SPLINE_CURVE((1.0000191574532,1.07458139657217,1.05821963517906))
REPRESENTATION_ITEM('')
);
#1137=(
BOUNDED_CURVE()
B_SPLINE_CURVE(2,(#25342,#25343,#25344),.UNSPECIFIED.,.F.,.F.)
B_SPLINE_CURVE_WITH_KNOTS((3,3),(2.06499351855609E-6,0.0443065724917911),
 .UNSPECIFIED.)
CURVE()
GEOMETRIC_REPRESENTATION_ITEM()
RATIONAL_B_SPLINE_CURVE((1.00000000159957,1.00001716071458,1.00002056801363))
REPRESENTATION_ITEM('')
);
#1138=(
BOUNDED_CURVE()
B_SPLINE_CURVE(2,(#25346,#25347,#25348),.UNSPECIFIED.,.F.,.F.)
B_SPLINE_CURVE_WITH_KNOTS((3,3),(0.0392023395450884,0.100434111321656),
 .UNSPECIFIED.)
CURVE()
GEOMETRIC_REPRESENTATION_ITEM()
RATIONAL_B_SPLINE_CURVE((1.05821963517918,1.07458139657233,1.00001915745319))
REPRESENTATION_ITEM('')
);
#1139=(
BOUNDED_CURVE()
B_SPLINE_CURVE(2,(#25354,#25355,#25356),.UNSPECIFIED.,.F.,.F.)
B_SPLINE_CURVE_WITH_KNOTS((3,3),(0.0142112171256352,0.110567648737535),
 .UNSPECIFIED.)
CURVE()
GEOMETRIC_REPRESENTATION_ITEM()
RATIONAL_B_SPLINE_CURVE((1.00000961767813,1.00003742650796,1.00000019074341))
REPRESENTATION_ITEM('')
);
#1140=(
BOUNDED_CURVE()
B_SPLINE_CURVE(2,(#25426,#25427,#25428),.UNSPECIFIED.,.F.,.F.)
B_SPLINE_CURVE_WITH_KNOTS((3,3),(0.0662606539244614,0.110565163369973),
 .UNSPECIFIED.)
CURVE()
GEOMETRIC_REPRESENTATION_ITEM()
RATIONAL_B_SPLINE_CURVE((1.00002056781072,1.00001716061294,1.00000000159956))
REPRESENTATION_ITEM('')
);
#1141=(
BOUNDED_CURVE()
B_SPLINE_CURVE(2,(#25435,#25436,#25437),.UNSPECIFIED.,.F.,.F.)
B_SPLINE_CURVE_WITH_KNOTS((3,3),(7.86559624220057E-6,0.0612396373727874),
 .UNSPECIFIED.)
CURVE()
GEOMETRIC_REPRESENTATION_ITEM()
RATIONAL_B_SPLINE_CURVE((1.00001915745323,1.07458139657226,1.05821963517912))
REPRESENTATION_ITEM('')
);
#1142=(
BOUNDED_CURVE()
B_SPLINE_CURVE(2,(#25442,#25443,#25444),.UNSPECIFIED.,.F.,.F.)
B_SPLINE_CURVE_WITH_KNOTS((3,3),(0.0392023395450873,0.100434111321653),
 .UNSPECIFIED.)
CURVE()
GEOMETRIC_REPRESENTATION_ITEM()
RATIONAL_B_SPLINE_CURVE((1.05821963517917,1.07458139657232,1.00001915745321))
REPRESENTATION_ITEM('')
);
#1143=(
BOUNDED_CURVE()
B_SPLINE_CURVE(2,(#25462,#25463,#25464),.UNSPECIFIED.,.F.,.F.)
B_SPLINE_CURVE_WITH_KNOTS((3,3),(2.06502885188068E-6,0.0443073288438163),
 .UNSPECIFIED.)
CURVE()
GEOMETRIC_REPRESENTATION_ITEM()
RATIONAL_B_SPLINE_CURVE((1.00000000159591,1.00001712140878,1.00002048940618))
REPRESENTATION_ITEM('')
);
#1144=(
BOUNDED_CURVE()
B_SPLINE_CURVE(2,(#25469,#25470,#25471),.UNSPECIFIED.,.F.,.F.)
B_SPLINE_CURVE_WITH_KNOTS((3,3),(0.0660091927116148,0.110314456526714),
 .UNSPECIFIED.)
CURVE()
GEOMETRIC_REPRESENTATION_ITEM()
RATIONAL_B_SPLINE_CURVE((1.00002048940315,1.00001712140625,1.00000000159591))
REPRESENTATION_ITEM('')
);
#1145=(
BOUNDED_CURVE()
B_SPLINE_CURVE(2,(#25483,#25484,#25485),.UNSPECIFIED.,.F.,.F.)
B_SPLINE_CURVE_WITH_KNOTS((3,3),(7.86559624218418E-6,0.0612396373727888),
 .UNSPECIFIED.)
CURVE()
GEOMETRIC_REPRESENTATION_ITEM()
RATIONAL_B_SPLINE_CURVE((1.00001915745323,1.07458139657228,1.05821963517914))
REPRESENTATION_ITEM('')
);
#1146=(
BOUNDED_CURVE()
B_SPLINE_CURVE(2,(#25490,#25491,#25492),.UNSPECIFIED.,.F.,.F.)
B_SPLINE_CURVE_WITH_KNOTS((3,3),(0.039202339545094,0.100434111321663),
 .UNSPECIFIED.)
CURVE()
GEOMETRIC_REPRESENTATION_ITEM()
RATIONAL_B_SPLINE_CURVE((1.05821963517907,1.07458139657219,1.00001915745321))
REPRESENTATION_ITEM('')
);
#1147=(
BOUNDED_CURVE()
B_SPLINE_CURVE(2,(#25506,#25507,#25508),.UNSPECIFIED.,.F.,.F.)
B_SPLINE_CURVE_WITH_KNOTS((3,3),(2.06502885290881E-6,0.0443073288438236),
 .UNSPECIFIED.)
CURVE()
GEOMETRIC_REPRESENTATION_ITEM()
RATIONAL_B_SPLINE_CURVE((1.00000000159591,1.0000171214084,1.00002048940573))
REPRESENTATION_ITEM('')
);
#1148=(
BOUNDED_CURVE()
B_SPLINE_CURVE(2,(#25512,#25513,#25514),.UNSPECIFIED.,.F.,.F.)
B_SPLINE_CURVE_WITH_KNOTS((3,3),(0.0660091927116525,0.110314456526715),
 .UNSPECIFIED.)
CURVE()
GEOMETRIC_REPRESENTATION_ITEM()
RATIONAL_B_SPLINE_CURVE((1.00002048941054,1.00001712141242,1.00000000159591))
REPRESENTATION_ITEM('')
);
#1149=(
BOUNDED_CURVE()
B_SPLINE_CURVE(2,(#25521,#25522,#25523),.UNSPECIFIED.,.F.,.F.)
B_SPLINE_CURVE_WITH_KNOTS((3,3),(7.86559624776651E-6,0.0612396373727933),
 .UNSPECIFIED.)
CURVE()
GEOMETRIC_REPRESENTATION_ITEM()
RATIONAL_B_SPLINE_CURVE((1.00001915745324,1.07458139657231,1.05821963517916))
REPRESENTATION_ITEM('')
);
#1150=(
BOUNDED_CURVE()
B_SPLINE_CURVE(2,(#25528,#25529,#25530),.UNSPECIFIED.,.F.,.F.)
B_SPLINE_CURVE_WITH_KNOTS((3,3),(0.0392023395450758,0.100434111321633),
 .UNSPECIFIED.)
CURVE()
GEOMETRIC_REPRESENTATION_ITEM()
RATIONAL_B_SPLINE_CURVE((1.05821963517916,1.07458139657231,1.00001915745321))
REPRESENTATION_ITEM('')
);
#1151=(
BOUNDED_CURVE()
B_SPLINE_CURVE(2,(#25548,#25549,#25550),.UNSPECIFIED.,.F.,.F.)
B_SPLINE_CURVE_WITH_KNOTS((3,3),(2.06502885179237E-6,0.0443073288439585),
 .UNSPECIFIED.)
CURVE()
GEOMETRIC_REPRESENTATION_ITEM()
RATIONAL_B_SPLINE_CURVE((1.00000000159591,1.00001712140818,1.00002048940547))
REPRESENTATION_ITEM('')
);
#1152=(
BOUNDED_CURVE()
B_SPLINE_CURVE(2,(#25554,#25555,#25556),.UNSPECIFIED.,.F.,.F.)
B_SPLINE_CURVE_WITH_KNOTS((3,3),(0.0660091927116068,0.110314456526714),
 .UNSPECIFIED.)
CURVE()
GEOMETRIC_REPRESENTATION_ITEM()
RATIONAL_B_SPLINE_CURVE((1.00002048940856,1.00001712141077,1.00000000159591))
REPRESENTATION_ITEM('')
);
#1153=(
BOUNDED_CURVE()
B_SPLINE_CURVE(2,(#25563,#25564,#25565),.UNSPECIFIED.,.F.,.F.)
B_SPLINE_CURVE_WITH_KNOTS((3,3),(7.86559623936065E-6,0.0612396373727857),
 .UNSPECIFIED.)
CURVE()
GEOMETRIC_REPRESENTATION_ITEM()
RATIONAL_B_SPLINE_CURVE((1.00001915745322,1.07458139657226,1.05821963517912))
REPRESENTATION_ITEM('')
);
#1154=(
BOUNDED_CURVE()
B_SPLINE_CURVE(2,(#25570,#25571,#25572),.UNSPECIFIED.,.F.,.F.)
B_SPLINE_CURVE_WITH_KNOTS((3,3),(0.0392023395450771,0.100434111321633),
 .UNSPECIFIED.)
CURVE()
GEOMETRIC_REPRESENTATION_ITEM()
RATIONAL_B_SPLINE_CURVE((1.05821963517909,1.07458139657222,1.00001915745321))
REPRESENTATION_ITEM('')
);
#1155=(
BOUNDED_CURVE()
B_SPLINE_CURVE(2,(#25588,#25589,#25590),.UNSPECIFIED.,.F.,.F.)
B_SPLINE_CURVE_WITH_KNOTS((3,3),(0.0142112171255719,0.110567648737547),
 .UNSPECIFIED.)
CURVE()
GEOMETRIC_REPRESENTATION_ITEM()
RATIONAL_B_SPLINE_CURVE((1.00000961768055,1.0000374265174,1.00000019074346))
REPRESENTATION_ITEM('')
);
#1156=(
BOUNDED_CURVE()
B_SPLINE_CURVE(2,(#25607,#25608,#25609),.UNSPECIFIED.,.F.,.F.)
B_SPLINE_CURVE_WITH_KNOTS((3,3),(0.000246247416175262,0.0445514940288951),
 .UNSPECIFIED.)
CURVE()
GEOMETRIC_REPRESENTATION_ITEM()
RATIONAL_B_SPLINE_CURVE((1.00000019074347,1.00001731196895,1.00002068137279))
REPRESENTATION_ITEM('')
);
#1157=(
BOUNDED_CURVE()
B_SPLINE_CURVE(2,(#25619,#25620,#25621),.UNSPECIFIED.,.F.,.F.)
B_SPLINE_CURVE_WITH_KNOTS((3,3),(0.00024624741617372,0.0966026790275413),
 .UNSPECIFIED.)
CURVE()
GEOMETRIC_REPRESENTATION_ITEM()
RATIONAL_B_SPLINE_CURVE((1.00000019074349,1.00003742652381,1.0000096176822))
REPRESENTATION_ITEM('')
);
#1158=(
BOUNDED_CURVE()
B_SPLINE_CURVE(2,(#25627,#25628,#25629),.UNSPECIFIED.,.F.,.F.)
B_SPLINE_CURVE_WITH_KNOTS((3,3),(0.0662624021246591,0.110567648737537),
 .UNSPECIFIED.)
CURVE()
GEOMETRIC_REPRESENTATION_ITEM()
RATIONAL_B_SPLINE_CURVE((1.00002068136771,1.0000173119647,1.00000019074342))
REPRESENTATION_ITEM('')
);
#1159=(
BOUNDED_CURVE()
B_SPLINE_CURVE(2,(#25647,#25648,#25649),.UNSPECIFIED.,.F.,.F.)
B_SPLINE_CURVE_WITH_KNOTS((3,3),(7.86559625117043E-6,0.0612396373728031),
 .UNSPECIFIED.)
CURVE()
GEOMETRIC_REPRESENTATION_ITEM()
RATIONAL_B_SPLINE_CURVE((1.00001915745325,1.07458139657221,1.05821963517909))
REPRESENTATION_ITEM('')
);
#1160=(
BOUNDED_CURVE()
B_SPLINE_CURVE(2,(#25657,#25658,#25659),.UNSPECIFIED.,.F.,.F.)
B_SPLINE_CURVE_WITH_KNOTS((3,3),(2.06502885156182E-6,0.0443073288437527),
 .UNSPECIFIED.)
CURVE()
GEOMETRIC_REPRESENTATION_ITEM()
RATIONAL_B_SPLINE_CURVE((1.00000000159591,1.00001712141345,1.00002048941177))
REPRESENTATION_ITEM('')
);
#1161=(
BOUNDED_CURVE()
B_SPLINE_CURVE(2,(#25661,#25662,#25663),.UNSPECIFIED.,.F.,.F.)
B_SPLINE_CURVE_WITH_KNOTS((3,3),(0.0392023395450928,0.100434111321662),
 .UNSPECIFIED.)
CURVE()
GEOMETRIC_REPRESENTATION_ITEM()
RATIONAL_B_SPLINE_CURVE((1.05821963517921,1.07458139657238,1.00001915745323))
REPRESENTATION_ITEM('')
);
#1162=(
BOUNDED_CURVE()
B_SPLINE_CURVE(2,(#25669,#25670,#25671),.UNSPECIFIED.,.F.,.F.)
B_SPLINE_CURVE_WITH_KNOTS((3,3),(0.0660091927115642,0.110314456526669),
 .UNSPECIFIED.)
CURVE()
GEOMETRIC_REPRESENTATION_ITEM()
RATIONAL_B_SPLINE_CURVE((1.00002048940194,1.00001712140523,1.00000000159591))
REPRESENTATION_ITEM('')
);
#1163=(
BOUNDED_CURVE()
B_SPLINE_CURVE(2,(#25689,#25690,#25691),.UNSPECIFIED.,.F.,.F.)
B_SPLINE_CURVE_WITH_KNOTS((3,3),(7.86559623322606E-6,0.0612396373727938),
 .UNSPECIFIED.)
CURVE()
GEOMETRIC_REPRESENTATION_ITEM()
RATIONAL_B_SPLINE_CURVE((1.0000191574532,1.07458139657236,1.05821963517921))
REPRESENTATION_ITEM('')
);
#1164=(
BOUNDED_CURVE()
B_SPLINE_CURVE(2,(#25699,#25700,#25701),.UNSPECIFIED.,.F.,.F.)
B_SPLINE_CURVE_WITH_KNOTS((3,3),(2.06502884885516E-6,0.0443073288438225),
 .UNSPECIFIED.)
CURVE()
GEOMETRIC_REPRESENTATION_ITEM()
RATIONAL_B_SPLINE_CURVE((1.00000000159591,1.00001712141336,1.00002048941166))
REPRESENTATION_ITEM('')
);
#1165=(
BOUNDED_CURVE()
B_SPLINE_CURVE(2,(#25703,#25704,#25705),.UNSPECIFIED.,.F.,.F.)
B_SPLINE_CURVE_WITH_KNOTS((3,3),(0.0392023395450786,0.100434111321634),
 .UNSPECIFIED.)
CURVE()
GEOMETRIC_REPRESENTATION_ITEM()
RATIONAL_B_SPLINE_CURVE((1.05821963517908,1.07458139657221,1.00001915745319))
REPRESENTATION_ITEM('')
);
#1166=(
BOUNDED_CURVE()
B_SPLINE_CURVE(2,(#25711,#25712,#25713),.UNSPECIFIED.,.F.,.F.)
B_SPLINE_CURVE_WITH_KNOTS((3,3),(0.0660091927118087,0.110314456526683),
 .UNSPECIFIED.)
CURVE()
GEOMETRIC_REPRESENTATION_ITEM()
RATIONAL_B_SPLINE_CURVE((1.00002048941584,1.00001712141684,1.00000000159591))
REPRESENTATION_ITEM('')
);
#1167=(
BOUNDED_CURVE()
B_SPLINE_CURVE(2,(#25731,#25732,#25733),.UNSPECIFIED.,.F.,.F.)
B_SPLINE_CURVE_WITH_KNOTS((3,3),(7.8655962357978E-6,0.061239637372792),
 .UNSPECIFIED.)
CURVE()
GEOMETRIC_REPRESENTATION_ITEM()
RATIONAL_B_SPLINE_CURVE((1.00001915745321,1.07458139657234,1.0582196351792))
REPRESENTATION_ITEM('')
);
#1168=(
BOUNDED_CURVE()
B_SPLINE_CURVE(2,(#25741,#25742,#25743),.UNSPECIFIED.,.F.,.F.)
B_SPLINE_CURVE_WITH_KNOTS((3,3),(2.06502885395743E-6,0.044307328843898),
 .UNSPECIFIED.)
CURVE()
GEOMETRIC_REPRESENTATION_ITEM()
RATIONAL_B_SPLINE_CURVE((1.00000000159591,1.00001712141084,1.00002048940865))
REPRESENTATION_ITEM('')
);
#1169=(
BOUNDED_CURVE()
B_SPLINE_CURVE(2,(#25745,#25746,#25747),.UNSPECIFIED.,.F.,.F.)
B_SPLINE_CURVE_WITH_KNOTS((3,3),(0.0392023395450774,0.100434111321634),
 .UNSPECIFIED.)
CURVE()
GEOMETRIC_REPRESENTATION_ITEM()
RATIONAL_B_SPLINE_CURVE((1.05821963517915,1.0745813965723,1.0000191574532))
REPRESENTATION_ITEM('')
);
#1170=(
BOUNDED_CURVE()
B_SPLINE_CURVE(2,(#25753,#25754,#25755),.UNSPECIFIED.,.F.,.F.)
B_SPLINE_CURVE_WITH_KNOTS((3,3),(0.0660091927117082,0.110314456526671),
 .UNSPECIFIED.)
CURVE()
GEOMETRIC_REPRESENTATION_ITEM()
RATIONAL_B_SPLINE_CURVE((1.00002048940984,1.00001712141184,1.00000000159591))
REPRESENTATION_ITEM('')
);
#1171=(
BOUNDED_CURVE()
B_SPLINE_CURVE(2,(#25773,#25774,#25775),.UNSPECIFIED.,.F.,.F.)
B_SPLINE_CURVE_WITH_KNOTS((3,3),(7.86559624864885E-6,0.0612396373728071),
 .UNSPECIFIED.)
CURVE()
GEOMETRIC_REPRESENTATION_ITEM()
RATIONAL_B_SPLINE_CURVE((1.00001915745324,1.07458139657234,1.05821963517919))
REPRESENTATION_ITEM('')
);
#1172=(
BOUNDED_CURVE()
B_SPLINE_CURVE(2,(#25783,#25784,#25785),.UNSPECIFIED.,.F.,.F.)
B_SPLINE_CURVE_WITH_KNOTS((3,3),(2.06499351570084E-6,0.0443065724918005),
 .UNSPECIFIED.)
CURVE()
GEOMETRIC_REPRESENTATION_ITEM()
RATIONAL_B_SPLINE_CURVE((1.00000000159957,1.00001716071775,1.00002056801743))
REPRESENTATION_ITEM('')
);
#1173=(
BOUNDED_CURVE()
B_SPLINE_CURVE(2,(#25787,#25788,#25789),.UNSPECIFIED.,.F.,.F.)
B_SPLINE_CURVE_WITH_KNOTS((3,3),(0.0392023395450912,0.100434111321662),
 .UNSPECIFIED.)
CURVE()
GEOMETRIC_REPRESENTATION_ITEM()
RATIONAL_B_SPLINE_CURVE((1.05821963517924,1.07458139657241,1.00001915745322))
REPRESENTATION_ITEM('')
);
#1174=(
BOUNDED_CURVE()
B_SPLINE_CURVE(2,(#25795,#25796,#25797),.UNSPECIFIED.,.F.,.F.)
B_SPLINE_CURVE_WITH_KNOTS((3,3),(0.0142112171255301,0.110567648737574),
 .UNSPECIFIED.)
CURVE()
GEOMETRIC_REPRESENTATION_ITEM()
RATIONAL_B_SPLINE_CURVE((1.00000961768267,1.00003742652563,1.0000001907435))
REPRESENTATION_ITEM('')
);
#1175=(
BOUNDED_CURVE()
B_SPLINE_CURVE(2,(#25865,#25866,#25867),.UNSPECIFIED.,.F.,.F.)
B_SPLINE_CURVE_WITH_KNOTS((3,3),(0.0662687847811601,0.110573269834452),
 .UNSPECIFIED.)
CURVE()
GEOMETRIC_REPRESENTATION_ITEM()
RATIONAL_B_SPLINE_CURVE((1.00002057034868,1.0000171618829,1.00000000159968))
REPRESENTATION_ITEM('')
);
#1176=(
BOUNDED_CURVE()
B_SPLINE_CURVE(2,(#25874,#25875,#25876),.UNSPECIFIED.,.F.,.F.)
B_SPLINE_CURVE_WITH_KNOTS((3,3),(7.86559624840906E-6,0.0612396373727937),
 .UNSPECIFIED.)
CURVE()
GEOMETRIC_REPRESENTATION_ITEM()
RATIONAL_B_SPLINE_CURVE((1.00001915745324,1.07458139657234,1.05821963517918))
REPRESENTATION_ITEM('')
);
#1177=(
BOUNDED_CURVE()
B_SPLINE_CURVE(2,(#25881,#25882,#25883),.UNSPECIFIED.,.F.,.F.)
B_SPLINE_CURVE_WITH_KNOTS((3,3),(0.0392023395450789,0.100434111321632),
 .UNSPECIFIED.)
CURVE()
GEOMETRIC_REPRESENTATION_ITEM()
RATIONAL_B_SPLINE_CURVE((1.05821963517911,1.07458139657224,1.00001915745322))
REPRESENTATION_ITEM('')
);
#1178=(
BOUNDED_CURVE()
B_SPLINE_CURVE(2,(#25901,#25902,#25903),.UNSPECIFIED.,.F.,.F.)
B_SPLINE_CURVE_WITH_KNOTS((3,3),(2.06502885157014E-6,0.0443073288439265),
 .UNSPECIFIED.)
CURVE()
GEOMETRIC_REPRESENTATION_ITEM()
RATIONAL_B_SPLINE_CURVE((1.00000000159591,1.00001712140936,1.00002048940688))
REPRESENTATION_ITEM('')
);
#1179=(
BOUNDED_CURVE()
B_SPLINE_CURVE(2,(#25907,#25908,#25909),.UNSPECIFIED.,.F.,.F.)
B_SPLINE_CURVE_WITH_KNOTS((3,3),(0.0660091927116283,0.110314456526686),
 .UNSPECIFIED.)
CURVE()
GEOMETRIC_REPRESENTATION_ITEM()
RATIONAL_B_SPLINE_CURVE((1.00002048940932,1.0000171214114,1.00000000159591))
REPRESENTATION_ITEM('')
);
#1180=(
BOUNDED_CURVE()
B_SPLINE_CURVE(2,(#25916,#25917,#25918),.UNSPECIFIED.,.F.,.F.)
B_SPLINE_CURVE_WITH_KNOTS((3,3),(7.86559624572803E-6,0.0612396373728016),
 .UNSPECIFIED.)
CURVE()
GEOMETRIC_REPRESENTATION_ITEM()
RATIONAL_B_SPLINE_CURVE((1.00001915745324,1.07458139657241,1.05821963517924))
REPRESENTATION_ITEM('')
);
#1181=(
BOUNDED_CURVE()
B_SPLINE_CURVE(2,(#25923,#25924,#25925),.UNSPECIFIED.,.F.,.F.)
B_SPLINE_CURVE_WITH_KNOTS((3,3),(0.0392023395450739,0.100434111321633),
 .UNSPECIFIED.)
CURVE()
GEOMETRIC_REPRESENTATION_ITEM()
RATIONAL_B_SPLINE_CURVE((1.05821963517925,1.07458139657243,1.00001915745321))
REPRESENTATION_ITEM('')
);
#1182=(
BOUNDED_CURVE()
B_SPLINE_CURVE(2,(#25943,#25944,#25945),.UNSPECIFIED.,.F.,.F.)
B_SPLINE_CURVE_WITH_KNOTS((3,3),(2.06502885149483E-6,0.0443073288439875),
 .UNSPECIFIED.)
CURVE()
GEOMETRIC_REPRESENTATION_ITEM()
RATIONAL_B_SPLINE_CURVE((1.00000000159591,1.00001712140408,1.00002048940056))
REPRESENTATION_ITEM('')
);
#1183=(
BOUNDED_CURVE()
B_SPLINE_CURVE(2,(#25949,#25950,#25951),.UNSPECIFIED.,.F.,.F.)
B_SPLINE_CURVE_WITH_KNOTS((3,3),(0.0660091927116748,0.110314456526719),
 .UNSPECIFIED.)
CURVE()
GEOMETRIC_REPRESENTATION_ITEM()
RATIONAL_B_SPLINE_CURVE((1.00002048940816,1.00001712141043,1.00000000159591))
REPRESENTATION_ITEM('')
);
#1184=(
BOUNDED_CURVE()
B_SPLINE_CURVE(2,(#25958,#25959,#25960),.UNSPECIFIED.,.F.,.F.)
B_SPLINE_CURVE_WITH_KNOTS((3,3),(7.86559623735724E-6,0.0612396373727826),
 .UNSPECIFIED.)
CURVE()
GEOMETRIC_REPRESENTATION_ITEM()
RATIONAL_B_SPLINE_CURVE((1.00001915745322,1.07458139657221,1.05821963517909))
REPRESENTATION_ITEM('')
);
#1185=(
BOUNDED_CURVE()
B_SPLINE_CURVE(2,(#25965,#25966,#25967),.UNSPECIFIED.,.F.,.F.)
B_SPLINE_CURVE_WITH_KNOTS((3,3),(0.03920233954508,0.100434111321635),
 .UNSPECIFIED.)
CURVE()
GEOMETRIC_REPRESENTATION_ITEM()
RATIONAL_B_SPLINE_CURVE((1.05821963517901,1.07458139657211,1.00001915745319))
REPRESENTATION_ITEM('')
);
#1186=(
BOUNDED_CURVE()
B_SPLINE_CURVE(2,(#25985,#25986,#25987),.UNSPECIFIED.,.F.,.F.)
B_SPLINE_CURVE_WITH_KNOTS((3,3),(2.06502885016307E-6,0.0443073288439128),
 .UNSPECIFIED.)
CURVE()
GEOMETRIC_REPRESENTATION_ITEM()
RATIONAL_B_SPLINE_CURVE((1.00000000159591,1.00001712140628,1.00002048940319))
REPRESENTATION_ITEM('')
);
#1187=(
BOUNDED_CURVE()
B_SPLINE_CURVE(2,(#25991,#25992,#25993),.UNSPECIFIED.,.F.,.F.)
B_SPLINE_CURVE_WITH_KNOTS((3,3),(0.0660091927116612,0.110314456526684),
 .UNSPECIFIED.)
CURVE()
GEOMETRIC_REPRESENTATION_ITEM()
RATIONAL_B_SPLINE_CURVE((1.0000204894059,1.00001712140854,1.00000000159591))
REPRESENTATION_ITEM('')
);
#1188=(
BOUNDED_CURVE()
B_SPLINE_CURVE(2,(#26000,#26001,#26002),.UNSPECIFIED.,.F.,.F.)
B_SPLINE_CURVE_WITH_KNOTS((3,3),(7.8655962337785E-6,0.0612396373727908),
 .UNSPECIFIED.)
CURVE()
GEOMETRIC_REPRESENTATION_ITEM()
RATIONAL_B_SPLINE_CURVE((1.00001915745321,1.0745813965724,1.05821963517924))
REPRESENTATION_ITEM('')
);
#1189=(
BOUNDED_CURVE()
B_SPLINE_CURVE(2,(#26007,#26008,#26009),.UNSPECIFIED.,.F.,.F.)
B_SPLINE_CURVE_WITH_KNOTS((3,3),(0.0392023395450855,0.100434111321653),
 .UNSPECIFIED.)
CURVE()
GEOMETRIC_REPRESENTATION_ITEM()
RATIONAL_B_SPLINE_CURVE((1.05821963517918,1.07458139657233,1.00001915745317))
REPRESENTATION_ITEM('')
);
#1190=(
BOUNDED_CURVE()
B_SPLINE_CURVE(2,(#26027,#26028,#26029),.UNSPECIFIED.,.F.,.F.)
B_SPLINE_CURVE_WITH_KNOTS((3,3),(2.06502884716521E-6,0.0443073288437792),
 .UNSPECIFIED.)
CURVE()
GEOMETRIC_REPRESENTATION_ITEM()
RATIONAL_B_SPLINE_CURVE((1.00000000159591,1.00001712141784,1.00002048941702))
REPRESENTATION_ITEM('')
);
#1191=(
BOUNDED_CURVE()
B_SPLINE_CURVE(2,(#26033,#26034,#26035),.UNSPECIFIED.,.F.,.F.)
B_SPLINE_CURVE_WITH_KNOTS((3,3),(0.0660091927116124,0.110314456526681),
 .UNSPECIFIED.)
CURVE()
GEOMETRIC_REPRESENTATION_ITEM()
RATIONAL_B_SPLINE_CURVE((1.00002048940556,1.00001712140826,1.00000000159591))
REPRESENTATION_ITEM('')
);
#1192=(
BOUNDED_CURVE()
B_SPLINE_CURVE(2,(#26042,#26043,#26044),.UNSPECIFIED.,.F.,.F.)
B_SPLINE_CURVE_WITH_KNOTS((3,3),(7.8655962373003E-6,0.0612396373727924),
 .UNSPECIFIED.)
CURVE()
GEOMETRIC_REPRESENTATION_ITEM()
RATIONAL_B_SPLINE_CURVE((1.00001915745321,1.07458139657233,1.05821963517918))
REPRESENTATION_ITEM('')
);
#1193=(
BOUNDED_CURVE()
B_SPLINE_CURVE(2,(#26049,#26050,#26051),.UNSPECIFIED.,.F.,.F.)
B_SPLINE_CURVE_WITH_KNOTS((3,3),(0.0392023395450769,0.100434111321635),
 .UNSPECIFIED.)
CURVE()
GEOMETRIC_REPRESENTATION_ITEM()
RATIONAL_B_SPLINE_CURVE((1.05821963517911,1.07458139657225,1.00001915745319))
REPRESENTATION_ITEM('')
);
#1194=(
BOUNDED_CURVE()
B_SPLINE_CURVE(2,(#26067,#26068,#26069),.UNSPECIFIED.,.F.,.F.)
B_SPLINE_CURVE_WITH_KNOTS((3,3),(0.0142112171257825,0.110567648737571),
 .UNSPECIFIED.)
CURVE()
GEOMETRIC_REPRESENTATION_ITEM()
RATIONAL_B_SPLINE_CURVE((1.00000961767676,1.00003742650262,1.00000019074339))
REPRESENTATION_ITEM('')
);
#1195=(
BOUNDED_CURVE()
B_SPLINE_CURVE(2,(#26086,#26087,#26088),.UNSPECIFIED.,.F.,.F.)
B_SPLINE_CURVE_WITH_KNOTS((3,3),(0.000246247416175026,0.0445514940289875),
 .UNSPECIFIED.)
CURVE()
GEOMETRIC_REPRESENTATION_ITEM()
RATIONAL_B_SPLINE_CURVE((1.0000001907434,1.00001731196304,1.00002068136573))
REPRESENTATION_ITEM('')
);
#1196=(
BOUNDED_CURVE()
B_SPLINE_CURVE(2,(#26098,#26099,#26100),.UNSPECIFIED.,.F.,.F.)
B_SPLINE_CURVE_WITH_KNOTS((3,3),(0.000246247416182682,0.0966026790274295),
 .UNSPECIFIED.)
CURVE()
GEOMETRIC_REPRESENTATION_ITEM()
RATIONAL_B_SPLINE_CURVE((1.00000019074342,1.00003742650901,1.0000096176784))
REPRESENTATION_ITEM('')
);
#1197=(
BOUNDED_CURVE()
B_SPLINE_CURVE(2,(#26106,#26107,#26108),.UNSPECIFIED.,.F.,.F.)
B_SPLINE_CURVE_WITH_KNOTS((3,3),(0.0662624021247521,0.110567648737547),
 .UNSPECIFIED.)
CURVE()
GEOMETRIC_REPRESENTATION_ITEM()
RATIONAL_B_SPLINE_CURVE((1.00002068137426,1.00001731197018,1.00000019074348))
REPRESENTATION_ITEM('')
);
#1198=(
BOUNDED_CURVE()
B_SPLINE_CURVE(2,(#26126,#26127,#26128),.UNSPECIFIED.,.F.,.F.)
B_SPLINE_CURVE_WITH_KNOTS((3,3),(7.86559623455466E-6,0.0612396373727871),
 .UNSPECIFIED.)
CURVE()
GEOMETRIC_REPRESENTATION_ITEM()
RATIONAL_B_SPLINE_CURVE((1.00001915745321,1.07458139657209,1.058219635179))
REPRESENTATION_ITEM('')
);
#1199=(
BOUNDED_CURVE()
B_SPLINE_CURVE(2,(#26136,#26137,#26138),.UNSPECIFIED.,.F.,.F.)
B_SPLINE_CURVE_WITH_KNOTS((3,3),(2.06502884828757E-6,0.0443073288439917),
 .UNSPECIFIED.)
CURVE()
GEOMETRIC_REPRESENTATION_ITEM()
RATIONAL_B_SPLINE_CURVE((1.00000000159591,1.00001712140454,1.00002048940111))
REPRESENTATION_ITEM('')
);
#1200=(
BOUNDED_CURVE()
B_SPLINE_CURVE(2,(#26140,#26141,#26142),.UNSPECIFIED.,.F.,.F.)
B_SPLINE_CURVE_WITH_KNOTS((3,3),(0.0392023395450789,0.100434111321635),
 .UNSPECIFIED.)
CURVE()
GEOMETRIC_REPRESENTATION_ITEM()
RATIONAL_B_SPLINE_CURVE((1.05821963517905,1.07458139657217,1.0000191574532))
REPRESENTATION_ITEM('')
);
#1201=(
BOUNDED_CURVE()
B_SPLINE_CURVE(2,(#26148,#26149,#26150),.UNSPECIFIED.,.F.,.F.)
B_SPLINE_CURVE_WITH_KNOTS((3,3),(0.0660091927117031,0.110314456526714),
 .UNSPECIFIED.)
CURVE()
GEOMETRIC_REPRESENTATION_ITEM()
RATIONAL_B_SPLINE_CURVE((1.00002048941073,1.00001712141258,1.00000000159591))
REPRESENTATION_ITEM('')
);
#1202=(
BOUNDED_CURVE()
B_SPLINE_CURVE(2,(#26168,#26169,#26170),.UNSPECIFIED.,.F.,.F.)
B_SPLINE_CURVE_WITH_KNOTS((3,3),(7.8655962436939E-6,0.0612396373727877),
 .UNSPECIFIED.)
CURVE()
GEOMETRIC_REPRESENTATION_ITEM()
RATIONAL_B_SPLINE_CURVE((1.00001915745323,1.07458139657225,1.05821963517912))
REPRESENTATION_ITEM('')
);
#1203=(
BOUNDED_CURVE()
B_SPLINE_CURVE(2,(#26178,#26179,#26180),.UNSPECIFIED.,.F.,.F.)
B_SPLINE_CURVE_WITH_KNOTS((3,3),(2.06502885453414E-6,0.0443073288439499),
 .UNSPECIFIED.)
CURVE()
GEOMETRIC_REPRESENTATION_ITEM()
RATIONAL_B_SPLINE_CURVE((1.00000000159591,1.00001712140702,1.00002048940408))
REPRESENTATION_ITEM('')
);
#1204=(
BOUNDED_CURVE()
B_SPLINE_CURVE(2,(#26182,#26183,#26184),.UNSPECIFIED.,.F.,.F.)
B_SPLINE_CURVE_WITH_KNOTS((3,3),(0.0392023395450765,0.100434111321633),
 .UNSPECIFIED.)
CURVE()
GEOMETRIC_REPRESENTATION_ITEM()
RATIONAL_B_SPLINE_CURVE((1.0582196351791,1.07458139657223,1.00001915745321))
REPRESENTATION_ITEM('')
);
#1205=(
BOUNDED_CURVE()
B_SPLINE_CURVE(2,(#26190,#26191,#26192),.UNSPECIFIED.,.F.,.F.)
B_SPLINE_CURVE_WITH_KNOTS((3,3),(0.0660091927116513,0.110314456526682),
 .UNSPECIFIED.)
CURVE()
GEOMETRIC_REPRESENTATION_ITEM()
RATIONAL_B_SPLINE_CURVE((1.00002048940269,1.00001712140586,1.00000000159591))
REPRESENTATION_ITEM('')
);
#1206=(
BOUNDED_CURVE()
B_SPLINE_CURVE(2,(#26210,#26211,#26212),.UNSPECIFIED.,.F.,.F.)
B_SPLINE_CURVE_WITH_KNOTS((3,3),(7.86559624777047E-6,0.0612396373728002),
 .UNSPECIFIED.)
CURVE()
GEOMETRIC_REPRESENTATION_ITEM()
RATIONAL_B_SPLINE_CURVE((1.00001915745324,1.0745813965723,1.05821963517915))
REPRESENTATION_ITEM('')
);
#1207=(
BOUNDED_CURVE()
B_SPLINE_CURVE(2,(#26220,#26221,#26222),.UNSPECIFIED.,.F.,.F.)
B_SPLINE_CURVE_WITH_KNOTS((3,3),(2.06499351625639E-6,0.0443065724919249),
 .UNSPECIFIED.)
CURVE()
GEOMETRIC_REPRESENTATION_ITEM()
RATIONAL_B_SPLINE_CURVE((1.00000000159957,1.00001716071701,1.00002056801654))
REPRESENTATION_ITEM('')
);
#1208=(
BOUNDED_CURVE()
B_SPLINE_CURVE(2,(#26224,#26225,#26226),.UNSPECIFIED.,.F.,.F.)
B_SPLINE_CURVE_WITH_KNOTS((3,3),(0.0392023395450864,0.100434111321651),
 .UNSPECIFIED.)
CURVE()
GEOMETRIC_REPRESENTATION_ITEM()
RATIONAL_B_SPLINE_CURVE((1.05821963517911,1.07458139657224,1.0000191574532))
REPRESENTATION_ITEM('')
);
#1209=(
BOUNDED_CURVE()
B_SPLINE_CURVE(2,(#26232,#26233,#26234),.UNSPECIFIED.,.F.,.F.)
B_SPLINE_CURVE_WITH_KNOTS((3,3),(0.0142112171256077,0.110567648737539),
 .UNSPECIFIED.)
CURVE()
GEOMETRIC_REPRESENTATION_ITEM()
RATIONAL_B_SPLINE_CURVE((1.00000961767965,1.00003742651388,1.00000019074344))
REPRESENTATION_ITEM('')
);
#1210=(
BOUNDED_CURVE()
B_SPLINE_CURVE(2,(#26304,#26305,#26306),.UNSPECIFIED.,.F.,.F.)
B_SPLINE_CURVE_WITH_KNOTS((3,3),(0.0662606539245541,0.110565163369947),
 .UNSPECIFIED.)
CURVE()
GEOMETRIC_REPRESENTATION_ITEM()
RATIONAL_B_SPLINE_CURVE((1.00002056780968,1.00001716061207,1.00000000159956))
REPRESENTATION_ITEM('')
);
#1211=(
BOUNDED_CURVE()
B_SPLINE_CURVE(2,(#26313,#26314,#26315),.UNSPECIFIED.,.F.,.F.)
B_SPLINE_CURVE_WITH_KNOTS((3,3),(7.86559623941073E-6,0.0612396373727952),
 .UNSPECIFIED.)
CURVE()
GEOMETRIC_REPRESENTATION_ITEM()
RATIONAL_B_SPLINE_CURVE((1.00001915745322,1.07458139657236,1.0582196351792))
REPRESENTATION_ITEM('')
);
#1212=(
BOUNDED_CURVE()
B_SPLINE_CURVE(2,(#26320,#26321,#26322),.UNSPECIFIED.,.F.,.F.)
B_SPLINE_CURVE_WITH_KNOTS((3,3),(0.0392023395450859,0.100434111321652),
 .UNSPECIFIED.)
CURVE()
GEOMETRIC_REPRESENTATION_ITEM()
RATIONAL_B_SPLINE_CURVE((1.05821963517913,1.07458139657226,1.0000191574532))
REPRESENTATION_ITEM('')
);
#1213=(
BOUNDED_CURVE()
B_SPLINE_CURVE(2,(#26340,#26341,#26342),.UNSPECIFIED.,.F.,.F.)
B_SPLINE_CURVE_WITH_KNOTS((3,3),(2.06502885201139E-6,0.0443073288438582),
 .UNSPECIFIED.)
CURVE()
GEOMETRIC_REPRESENTATION_ITEM()
RATIONAL_B_SPLINE_CURVE((1.00000000159591,1.00001712141177,1.00002048940977))
REPRESENTATION_ITEM('')
);
#1214=(
BOUNDED_CURVE()
B_SPLINE_CURVE(2,(#26347,#26348,#26349),.UNSPECIFIED.,.F.,.F.)
B_SPLINE_CURVE_WITH_KNOTS((3,3),(0.0660091927115239,0.110314456526711),
 .UNSPECIFIED.)
CURVE()
GEOMETRIC_REPRESENTATION_ITEM()
RATIONAL_B_SPLINE_CURVE((1.00002048939877,1.00001712140258,1.00000000159591))
REPRESENTATION_ITEM('')
);
#1215=(
BOUNDED_CURVE()
B_SPLINE_CURVE(2,(#26361,#26362,#26363),.UNSPECIFIED.,.F.,.F.)
B_SPLINE_CURVE_WITH_KNOTS((3,3),(7.86559624532228E-6,0.0612396373727895),
 .UNSPECIFIED.)
CURVE()
GEOMETRIC_REPRESENTATION_ITEM()
RATIONAL_B_SPLINE_CURVE((1.00001915745323,1.07458139657214,1.05821963517903))
REPRESENTATION_ITEM('')
);
#1216=(
BOUNDED_CURVE()
B_SPLINE_CURVE(2,(#26368,#26369,#26370),.UNSPECIFIED.,.F.,.F.)
B_SPLINE_CURVE_WITH_KNOTS((3,3),(0.0392023395450881,0.100434111321656),
 .UNSPECIFIED.)
CURVE()
GEOMETRIC_REPRESENTATION_ITEM()
RATIONAL_B_SPLINE_CURVE((1.05821963517912,1.07458139657226,1.00001915745319))
REPRESENTATION_ITEM('')
);
#1217=(
BOUNDED_CURVE()
B_SPLINE_CURVE(2,(#26384,#26385,#26386),.UNSPECIFIED.,.F.,.F.)
B_SPLINE_CURVE_WITH_KNOTS((3,3),(2.06502884911628E-6,0.0443073288438737),
 .UNSPECIFIED.)
CURVE()
GEOMETRIC_REPRESENTATION_ITEM()
RATIONAL_B_SPLINE_CURVE((1.00000000159591,1.00001712140897,1.00002048940641))
REPRESENTATION_ITEM('')
);
#1218=(
BOUNDED_CURVE()
B_SPLINE_CURVE(2,(#26390,#26391,#26392),.UNSPECIFIED.,.F.,.F.)
B_SPLINE_CURVE_WITH_KNOTS((3,3),(0.0660091927116664,0.110314456526713),
 .UNSPECIFIED.)
CURVE()
GEOMETRIC_REPRESENTATION_ITEM()
RATIONAL_B_SPLINE_CURVE((1.0000204894019,1.0000171214052,1.00000000159591))
REPRESENTATION_ITEM('')
);
#1219=(
BOUNDED_CURVE()
B_SPLINE_CURVE(2,(#26399,#26400,#26401),.UNSPECIFIED.,.F.,.F.)
B_SPLINE_CURVE_WITH_KNOTS((3,3),(7.86559624159626E-6,0.0612396373727846),
 .UNSPECIFIED.)
CURVE()
GEOMETRIC_REPRESENTATION_ITEM()
RATIONAL_B_SPLINE_CURVE((1.00001915745323,1.07458139657216,1.05821963517905))
REPRESENTATION_ITEM('')
);
#1220=(
BOUNDED_CURVE()
B_SPLINE_CURVE(2,(#26406,#26407,#26408),.UNSPECIFIED.,.F.,.F.)
B_SPLINE_CURVE_WITH_KNOTS((3,3),(0.0392023395450783,0.100434111321637),
 .UNSPECIFIED.)
CURVE()
GEOMETRIC_REPRESENTATION_ITEM()
RATIONAL_B_SPLINE_CURVE((1.05821963517912,1.07458139657226,1.00001915745319))
REPRESENTATION_ITEM('')
);
#1221=(
BOUNDED_CURVE()
B_SPLINE_CURVE(2,(#26426,#26427,#26428),.UNSPECIFIED.,.F.,.F.)
B_SPLINE_CURVE_WITH_KNOTS((3,3),(2.06502885183502E-6,0.0443073288439655),
 .UNSPECIFIED.)
CURVE()
GEOMETRIC_REPRESENTATION_ITEM()
RATIONAL_B_SPLINE_CURVE((1.00000000159591,1.00001712140387,1.00002048940031))
REPRESENTATION_ITEM('')
);
#1222=(
BOUNDED_CURVE()
B_SPLINE_CURVE(2,(#26432,#26433,#26434),.UNSPECIFIED.,.F.,.F.)
B_SPLINE_CURVE_WITH_KNOTS((3,3),(0.0660091927116195,0.110314456526666),
 .UNSPECIFIED.)
CURVE()
GEOMETRIC_REPRESENTATION_ITEM()
RATIONAL_B_SPLINE_CURVE((1.00002048940356,1.00001712140659,1.00000000159591))
REPRESENTATION_ITEM('')
);
#1223=(
BOUNDED_CURVE()
B_SPLINE_CURVE(2,(#26441,#26442,#26443),.UNSPECIFIED.,.F.,.F.)
B_SPLINE_CURVE_WITH_KNOTS((3,3),(7.8655962358422E-6,0.0612396373727976),
 .UNSPECIFIED.)
CURVE()
GEOMETRIC_REPRESENTATION_ITEM()
RATIONAL_B_SPLINE_CURVE((1.00001915745321,1.07458139657234,1.05821963517919))
REPRESENTATION_ITEM('')
);
#1224=(
BOUNDED_CURVE()
B_SPLINE_CURVE(2,(#26448,#26449,#26450),.UNSPECIFIED.,.F.,.F.)
B_SPLINE_CURVE_WITH_KNOTS((3,3),(0.0392023395450768,0.100434111321634),
 .UNSPECIFIED.)
CURVE()
GEOMETRIC_REPRESENTATION_ITEM()
RATIONAL_B_SPLINE_CURVE((1.0582196351792,1.07458139657236,1.00001915745321))
REPRESENTATION_ITEM('')
);
#1225=(
BOUNDED_CURVE()
B_SPLINE_CURVE(2,(#26468,#26469,#26470),.UNSPECIFIED.,.F.,.F.)
B_SPLINE_CURVE_WITH_KNOTS((3,3),(2.06502884978542E-6,0.044307328843927),
 .UNSPECIFIED.)
CURVE()
GEOMETRIC_REPRESENTATION_ITEM()
RATIONAL_B_SPLINE_CURVE((1.00000000159591,1.00001712141206,1.00002048941012))
REPRESENTATION_ITEM('')
);
#1226=(
BOUNDED_CURVE()
B_SPLINE_CURVE(2,(#26474,#26475,#26476),.UNSPECIFIED.,.F.,.F.)
B_SPLINE_CURVE_WITH_KNOTS((3,3),(0.0660091927117639,0.110314456526716),
 .UNSPECIFIED.)
CURVE()
GEOMETRIC_REPRESENTATION_ITEM()
RATIONAL_B_SPLINE_CURVE((1.00002048941328,1.00001712141471,1.00000000159591))
REPRESENTATION_ITEM('')
);
#1227=(
BOUNDED_CURVE()
B_SPLINE_CURVE(2,(#26483,#26484,#26485),.UNSPECIFIED.,.F.,.F.)
B_SPLINE_CURVE_WITH_KNOTS((3,3),(7.86559624401459E-6,0.061239637372789),
 .UNSPECIFIED.)
CURVE()
GEOMETRIC_REPRESENTATION_ITEM()
RATIONAL_B_SPLINE_CURVE((1.00001915745323,1.07458139657231,1.05821963517916))
REPRESENTATION_ITEM('')
);
#1228=(
BOUNDED_CURVE()
B_SPLINE_CURVE(2,(#26490,#26491,#26492),.UNSPECIFIED.,.F.,.F.)
B_SPLINE_CURVE_WITH_KNOTS((3,3),(0.0392023395450879,0.100434111321656),
 .UNSPECIFIED.)
CURVE()
GEOMETRIC_REPRESENTATION_ITEM()
RATIONAL_B_SPLINE_CURVE((1.05821963517917,1.07458139657232,1.00001915745319))
REPRESENTATION_ITEM('')
);
#1229=(
BOUNDED_CURVE()
B_SPLINE_CURVE(2,(#26510,#26511,#26512),.UNSPECIFIED.,.F.,.F.)
B_SPLINE_CURVE_WITH_KNOTS((3,3),(2.06502884833352E-6,0.044307328843929),
 .UNSPECIFIED.)
CURVE()
GEOMETRIC_REPRESENTATION_ITEM()
RATIONAL_B_SPLINE_CURVE((1.00000000159591,1.00001712141061,1.00002048940837))
REPRESENTATION_ITEM('')
);
#1230=(
BOUNDED_CURVE()
B_SPLINE_CURVE(2,(#26516,#26517,#26518),.UNSPECIFIED.,.F.,.F.)
B_SPLINE_CURVE_WITH_KNOTS((3,3),(0.0660091927116832,0.110314456526714),
 .UNSPECIFIED.)
CURVE()
GEOMETRIC_REPRESENTATION_ITEM()
RATIONAL_B_SPLINE_CURVE((1.00002048940784,1.00001712141016,1.00000000159591))
REPRESENTATION_ITEM('')
);
#1231=(
BOUNDED_CURVE()
B_SPLINE_CURVE(2,(#26525,#26526,#26527),.UNSPECIFIED.,.F.,.F.)
B_SPLINE_CURVE_WITH_KNOTS((3,3),(7.86559624514939E-6,0.0612396373727892),
 .UNSPECIFIED.)
CURVE()
GEOMETRIC_REPRESENTATION_ITEM()
RATIONAL_B_SPLINE_CURVE((1.00001915745323,1.07458139657222,1.05821963517909))
REPRESENTATION_ITEM('')
);
#1232=(
BOUNDED_CURVE()
B_SPLINE_CURVE(2,(#26532,#26533,#26534),.UNSPECIFIED.,.F.,.F.)
B_SPLINE_CURVE_WITH_KNOTS((3,3),(0.0392023395450942,0.100434111321667),
 .UNSPECIFIED.)
CURVE()
GEOMETRIC_REPRESENTATION_ITEM()
RATIONAL_B_SPLINE_CURVE((1.05821963517916,1.0745813965723,1.00001915745317))
REPRESENTATION_ITEM('')
);
#1233=(
BOUNDED_CURVE()
B_SPLINE_CURVE(2,(#26550,#26551,#26552),.UNSPECIFIED.,.F.,.F.)
B_SPLINE_CURVE_WITH_KNOTS((3,3),(0.0142193842176284,0.11057581462524),
 .UNSPECIFIED.)
CURVE()
GEOMETRIC_REPRESENTATION_ITEM()
RATIONAL_B_SPLINE_CURVE((1.00000962398904,1.00003743271758,1.00000019685764))
REPRESENTATION_ITEM('')
);
#1234=(
BOUNDED_CURVE()
B_SPLINE_CURVE(2,(#26569,#26570,#26571),.UNSPECIFIED.,.F.,.F.)
B_SPLINE_CURVE_WITH_KNOTS((3,3),(0.000254122058504862,0.0445593681152428),
 .UNSPECIFIED.)
CURVE()
GEOMETRIC_REPRESENTATION_ITEM()
RATIONAL_B_SPLINE_CURVE((1.00000019685769,1.0000173181266,1.00002068757546))
REPRESENTATION_ITEM('')
);
#1235=(
BOUNDED_CURVE()
B_SPLINE_CURVE(2,(#26581,#26582,#26583),.UNSPECIFIED.,.F.,.F.)
B_SPLINE_CURVE_WITH_KNOTS((3,3),(0.000246247416175252,0.0966026790274265),
 .UNSPECIFIED.)
CURVE()
GEOMETRIC_REPRESENTATION_ITEM()
RATIONAL_B_SPLINE_CURVE((1.00000019074343,1.00003742651156,1.00000961767906))
REPRESENTATION_ITEM('')
);
#1236=(
BOUNDED_CURVE()
B_SPLINE_CURVE(2,(#26589,#26590,#26591),.UNSPECIFIED.,.F.,.F.)
B_SPLINE_CURVE_WITH_KNOTS((3,3),(0.0662624021247102,0.11056764873757),
 .UNSPECIFIED.)
CURVE()
GEOMETRIC_REPRESENTATION_ITEM()
RATIONAL_B_SPLINE_CURVE((1.00002068136862,1.00001731196546,1.00000019074343))
REPRESENTATION_ITEM('')
);
#1237=(
BOUNDED_CURVE()
B_SPLINE_CURVE(2,(#26609,#26610,#26611),.UNSPECIFIED.,.F.,.F.)
B_SPLINE_CURVE_WITH_KNOTS((3,3),(7.86559623933804E-6,0.0612396373727864),
 .UNSPECIFIED.)
CURVE()
GEOMETRIC_REPRESENTATION_ITEM()
RATIONAL_B_SPLINE_CURVE((1.00001915745322,1.07458139657227,1.05821963517913))
REPRESENTATION_ITEM('')
);
#1238=(
BOUNDED_CURVE()
B_SPLINE_CURVE(2,(#26619,#26620,#26621),.UNSPECIFIED.,.F.,.F.)
B_SPLINE_CURVE_WITH_KNOTS((3,3),(2.06502885193672E-6,0.0443073288438289),
 .UNSPECIFIED.)
CURVE()
GEOMETRIC_REPRESENTATION_ITEM()
RATIONAL_B_SPLINE_CURVE((1.00000000159591,1.00001712141026,1.00002048940795))
REPRESENTATION_ITEM('')
);
#1239=(
BOUNDED_CURVE()
B_SPLINE_CURVE(2,(#26623,#26624,#26625),.UNSPECIFIED.,.F.,.F.)
B_SPLINE_CURVE_WITH_KNOTS((3,3),(0.0392023395450853,0.10043411132165),
 .UNSPECIFIED.)
CURVE()
GEOMETRIC_REPRESENTATION_ITEM()
RATIONAL_B_SPLINE_CURVE((1.05821963517918,1.07458139657234,1.00001915745322))
REPRESENTATION_ITEM('')
);
#1240=(
BOUNDED_CURVE()
B_SPLINE_CURVE(2,(#26631,#26632,#26633),.UNSPECIFIED.,.F.,.F.)
B_SPLINE_CURVE_WITH_KNOTS((3,3),(0.0660091927116699,0.110314456526683),
 .UNSPECIFIED.)
CURVE()
GEOMETRIC_REPRESENTATION_ITEM()
RATIONAL_B_SPLINE_CURVE((1.00002048940987,1.00001712141186,1.00000000159591))
REPRESENTATION_ITEM('')
);
#1241=(
BOUNDED_CURVE()
B_SPLINE_CURVE(2,(#26651,#26652,#26653),.UNSPECIFIED.,.F.,.F.)
B_SPLINE_CURVE_WITH_KNOTS((3,3),(7.86559624078655E-6,0.061239637372796),
 .UNSPECIFIED.)
CURVE()
GEOMETRIC_REPRESENTATION_ITEM()
RATIONAL_B_SPLINE_CURVE((1.00001915745322,1.07458139657237,1.05821963517922))
REPRESENTATION_ITEM('')
);
#1242=(
BOUNDED_CURVE()
B_SPLINE_CURVE(2,(#26661,#26662,#26663),.UNSPECIFIED.,.F.,.F.)
B_SPLINE_CURVE_WITH_KNOTS((3,3),(2.06499351893339E-6,0.0443065724918821),
 .UNSPECIFIED.)
CURVE()
GEOMETRIC_REPRESENTATION_ITEM()
RATIONAL_B_SPLINE_CURVE((1.00000000159957,1.0000171607139,1.00002056801282))
REPRESENTATION_ITEM('')
);
#1243=(
BOUNDED_CURVE()
B_SPLINE_CURVE(2,(#26665,#26666,#26667),.UNSPECIFIED.,.F.,.F.)
B_SPLINE_CURVE_WITH_KNOTS((3,3),(0.0392023395450775,0.100434111321634),
 .UNSPECIFIED.)
CURVE()
GEOMETRIC_REPRESENTATION_ITEM()
RATIONAL_B_SPLINE_CURVE((1.05821963517913,1.07458139657227,1.0000191574532))
REPRESENTATION_ITEM('')
);
#1244=(
BOUNDED_CURVE()
B_SPLINE_CURVE(2,(#26673,#26674,#26675),.UNSPECIFIED.,.F.,.F.)
B_SPLINE_CURVE_WITH_KNOTS((3,3),(0.0142112171257224,0.11056764873754),
 .UNSPECIFIED.)
CURVE()
GEOMETRIC_REPRESENTATION_ITEM()
RATIONAL_B_SPLINE_CURVE((1.00000961767654,1.00003742650177,1.00000019074338))
REPRESENTATION_ITEM('')
);
#1245=(
BOUNDED_CURVE()
B_SPLINE_CURVE(2,(#26743,#26744,#26745),.UNSPECIFIED.,.F.,.F.)
B_SPLINE_CURVE_WITH_KNOTS((3,3),(0.0662687847811842,0.110573269834456),
 .UNSPECIFIED.)
CURVE()
GEOMETRIC_REPRESENTATION_ITEM()
RATIONAL_B_SPLINE_CURVE((1.00002057034848,1.00001716188273,1.00000000159968))
REPRESENTATION_ITEM('')
);
#1246=(
BOUNDED_CURVE()
B_SPLINE_CURVE(2,(#26752,#26753,#26754),.UNSPECIFIED.,.F.,.F.)
B_SPLINE_CURVE_WITH_KNOTS((3,3),(7.86559623619297E-6,0.06123963737278),
 .UNSPECIFIED.)
CURVE()
GEOMETRIC_REPRESENTATION_ITEM()
RATIONAL_B_SPLINE_CURVE((1.00001915745321,1.0745813965721,1.058219635179))
REPRESENTATION_ITEM('')
);
#1247=(
BOUNDED_CURVE()
B_SPLINE_CURVE(2,(#26759,#26760,#26761),.UNSPECIFIED.,.F.,.F.)
B_SPLINE_CURVE_WITH_KNOTS((3,3),(0.039202339545078,0.100434111321636),
 .UNSPECIFIED.)
CURVE()
GEOMETRIC_REPRESENTATION_ITEM()
RATIONAL_B_SPLINE_CURVE((1.05821963517909,1.07458139657222,1.0000191574532))
REPRESENTATION_ITEM('')
);
#1248=(
BOUNDED_CURVE()
B_SPLINE_CURVE(2,(#26779,#26780,#26781),.UNSPECIFIED.,.F.,.F.)
B_SPLINE_CURVE_WITH_KNOTS((3,3),(2.06502885056018E-6,0.0443073288440188),
 .UNSPECIFIED.)
CURVE()
GEOMETRIC_REPRESENTATION_ITEM()
RATIONAL_B_SPLINE_CURVE((1.00000000159591,1.00001712140584,1.00002048940267))
REPRESENTATION_ITEM('')
);
#1249=(
BOUNDED_CURVE()
B_SPLINE_CURVE(2,(#26785,#26786,#26787),.UNSPECIFIED.,.F.,.F.)
B_SPLINE_CURVE_WITH_KNOTS((3,3),(0.0660091927117243,0.110314456526684),
 .UNSPECIFIED.)
CURVE()
GEOMETRIC_REPRESENTATION_ITEM()
RATIONAL_B_SPLINE_CURVE((1.00002048940642,1.00001712140897,1.00000000159591))
REPRESENTATION_ITEM('')
);
#1250=(
BOUNDED_CURVE()
B_SPLINE_CURVE(2,(#26794,#26795,#26796),.UNSPECIFIED.,.F.,.F.)
B_SPLINE_CURVE_WITH_KNOTS((3,3),(7.86559624052001E-6,0.0612396373727947),
 .UNSPECIFIED.)
CURVE()
GEOMETRIC_REPRESENTATION_ITEM()
RATIONAL_B_SPLINE_CURVE((1.00001915745322,1.0745813965723,1.05821963517916))
REPRESENTATION_ITEM('')
);
#1251=(
BOUNDED_CURVE()
B_SPLINE_CURVE(2,(#26801,#26802,#26803),.UNSPECIFIED.,.F.,.F.)
B_SPLINE_CURVE_WITH_KNOTS((3,3),(0.0392023395450857,0.100434111321653),
 .UNSPECIFIED.)
CURVE()
GEOMETRIC_REPRESENTATION_ITEM()
RATIONAL_B_SPLINE_CURVE((1.05821963517924,1.0745813965724,1.0000191574532))
REPRESENTATION_ITEM('')
);
#1252=(
BOUNDED_CURVE()
B_SPLINE_CURVE(2,(#26821,#26822,#26823),.UNSPECIFIED.,.F.,.F.)
B_SPLINE_CURVE_WITH_KNOTS((3,3),(2.0650288503503E-6,0.0443073288439064),
 .UNSPECIFIED.)
CURVE()
GEOMETRIC_REPRESENTATION_ITEM()
RATIONAL_B_SPLINE_CURVE((1.00000000159591,1.00001712140843,1.00002048940577))
REPRESENTATION_ITEM('')
);
#1253=(
BOUNDED_CURVE()
B_SPLINE_CURVE(2,(#26827,#26828,#26829),.UNSPECIFIED.,.F.,.F.)
B_SPLINE_CURVE_WITH_KNOTS((3,3),(0.0660091927115479,0.110314456526717),
 .UNSPECIFIED.)
CURVE()
GEOMETRIC_REPRESENTATION_ITEM()
RATIONAL_B_SPLINE_CURVE((1.00002048940187,1.00001712140517,1.00000000159591))
REPRESENTATION_ITEM('')
);
#1254=(
BOUNDED_CURVE()
B_SPLINE_CURVE(2,(#26836,#26837,#26838),.UNSPECIFIED.,.F.,.F.)
B_SPLINE_CURVE_WITH_KNOTS((3,3),(7.86559623675799E-6,0.0612396373727838),
 .UNSPECIFIED.)
CURVE()
GEOMETRIC_REPRESENTATION_ITEM()
RATIONAL_B_SPLINE_CURVE((1.00001915745321,1.07458139657228,1.05821963517914))
REPRESENTATION_ITEM('')
);
#1255=(
BOUNDED_CURVE()
B_SPLINE_CURVE(2,(#26843,#26844,#26845),.UNSPECIFIED.,.F.,.F.)
B_SPLINE_CURVE_WITH_KNOTS((3,3),(0.0392023395450765,0.100434111321632),
 .UNSPECIFIED.)
CURVE()
GEOMETRIC_REPRESENTATION_ITEM()
RATIONAL_B_SPLINE_CURVE((1.05821963517912,1.07458139657226,1.00001915745321))
REPRESENTATION_ITEM('')
);
#1256=(
BOUNDED_CURVE()
B_SPLINE_CURVE(2,(#26863,#26864,#26865),.UNSPECIFIED.,.F.,.F.)
B_SPLINE_CURVE_WITH_KNOTS((3,3),(2.06502885377429E-6,0.0443073288438915),
 .UNSPECIFIED.)
CURVE()
GEOMETRIC_REPRESENTATION_ITEM()
RATIONAL_B_SPLINE_CURVE((1.00000000159591,1.00001712141336,1.00002048941167))
REPRESENTATION_ITEM('')
);
#1257=(
BOUNDED_CURVE()
B_SPLINE_CURVE(2,(#26869,#26870,#26871),.UNSPECIFIED.,.F.,.F.)
B_SPLINE_CURVE_WITH_KNOTS((3,3),(0.0660091927116458,0.110314456526714),
 .UNSPECIFIED.)
CURVE()
GEOMETRIC_REPRESENTATION_ITEM()
RATIONAL_B_SPLINE_CURVE((1.000020489408,1.0000171214103,1.00000000159591))
REPRESENTATION_ITEM('')
);
#1258=(
BOUNDED_CURVE()
B_SPLINE_CURVE(2,(#26878,#26879,#26880),.UNSPECIFIED.,.F.,.F.)
B_SPLINE_CURVE_WITH_KNOTS((3,3),(7.86559625794864E-6,0.0612396373728014),
 .UNSPECIFIED.)
CURVE()
GEOMETRIC_REPRESENTATION_ITEM()
RATIONAL_B_SPLINE_CURVE((1.00001915745327,1.07458139657237,1.0582196351792))
REPRESENTATION_ITEM('')
);
#1259=(
BOUNDED_CURVE()
B_SPLINE_CURVE(2,(#26885,#26886,#26887),.UNSPECIFIED.,.F.,.F.)
B_SPLINE_CURVE_WITH_KNOTS((3,3),(0.0392023395450741,0.100434111321631),
 .UNSPECIFIED.)
CURVE()
GEOMETRIC_REPRESENTATION_ITEM()
RATIONAL_B_SPLINE_CURVE((1.05821963517911,1.07458139657226,1.00001915745322))
REPRESENTATION_ITEM('')
);
#1260=(
BOUNDED_CURVE()
B_SPLINE_CURVE(2,(#26905,#26906,#26907),.UNSPECIFIED.,.F.,.F.)
B_SPLINE_CURVE_WITH_KNOTS((3,3),(2.0650288534097E-6,0.0443073288438614),
 .UNSPECIFIED.)
CURVE()
GEOMETRIC_REPRESENTATION_ITEM()
RATIONAL_B_SPLINE_CURVE((1.00000000159591,1.00001712141325,1.00002048941153))
REPRESENTATION_ITEM('')
);
#1261=(
BOUNDED_CURVE()
B_SPLINE_CURVE(2,(#26911,#26912,#26913),.UNSPECIFIED.,.F.,.F.)
B_SPLINE_CURVE_WITH_KNOTS((3,3),(0.0660091927116462,0.110314456526715),
 .UNSPECIFIED.)
CURVE()
GEOMETRIC_REPRESENTATION_ITEM()
RATIONAL_B_SPLINE_CURVE((1.00002048940619,1.00001712140878,1.00000000159591))
REPRESENTATION_ITEM('')
);
#1262=(
BOUNDED_CURVE()
B_SPLINE_CURVE(2,(#26920,#26921,#26922),.UNSPECIFIED.,.F.,.F.)
B_SPLINE_CURVE_WITH_KNOTS((3,3),(7.86559624534418E-6,0.0612396373727898),
 .UNSPECIFIED.)
CURVE()
GEOMETRIC_REPRESENTATION_ITEM()
RATIONAL_B_SPLINE_CURVE((1.00001915745323,1.07458139657225,1.05821963517912))
REPRESENTATION_ITEM('')
);
#1263=(
BOUNDED_CURVE()
B_SPLINE_CURVE(2,(#26927,#26928,#26929),.UNSPECIFIED.,.F.,.F.)
B_SPLINE_CURVE_WITH_KNOTS((3,3),(0.039202339545079,0.100434111321632),
 .UNSPECIFIED.)
CURVE()
GEOMETRIC_REPRESENTATION_ITEM()
RATIONAL_B_SPLINE_CURVE((1.05821963517908,1.0745813965722,1.00001915745321))
REPRESENTATION_ITEM('')
);
#1264=(
BOUNDED_CURVE()
B_SPLINE_CURVE(2,(#26947,#26948,#26949),.UNSPECIFIED.,.F.,.F.)
B_SPLINE_CURVE_WITH_KNOTS((3,3),(2.06502885096946E-6,0.0443073288439515),
 .UNSPECIFIED.)
CURVE()
GEOMETRIC_REPRESENTATION_ITEM()
RATIONAL_B_SPLINE_CURVE((1.00000000159591,1.00001712140919,1.00002048940668))
REPRESENTATION_ITEM('')
);
#1265=(
BOUNDED_CURVE()
B_SPLINE_CURVE(2,(#26953,#26954,#26955),.UNSPECIFIED.,.F.,.F.)
B_SPLINE_CURVE_WITH_KNOTS((3,3),(0.0660091927116946,0.110314456526713),
 .UNSPECIFIED.)
CURVE()
GEOMETRIC_REPRESENTATION_ITEM()
RATIONAL_B_SPLINE_CURVE((1.00002048940625,1.00001712140884,1.00000000159591))
REPRESENTATION_ITEM('')
);
#1266=(
BOUNDED_CURVE()
B_SPLINE_CURVE(2,(#26962,#26963,#26964),.UNSPECIFIED.,.F.,.F.)
B_SPLINE_CURVE_WITH_KNOTS((3,3),(7.86559624800839E-6,0.0612396373727904),
 .UNSPECIFIED.)
CURVE()
GEOMETRIC_REPRESENTATION_ITEM()
RATIONAL_B_SPLINE_CURVE((1.00001915745324,1.07458139657215,1.05821963517904))
REPRESENTATION_ITEM('')
);
#1267=(
BOUNDED_CURVE()
B_SPLINE_CURVE(2,(#26969,#26970,#26971),.UNSPECIFIED.,.F.,.F.)
B_SPLINE_CURVE_WITH_KNOTS((3,3),(0.0392023395450754,0.100434111321632),
 .UNSPECIFIED.)
CURVE()
GEOMETRIC_REPRESENTATION_ITEM()
RATIONAL_B_SPLINE_CURVE((1.05821963517914,1.07458139657228,1.00001915745321))
REPRESENTATION_ITEM('')
);
#1268=(
BOUNDED_CURVE()
B_SPLINE_CURVE(2,(#26989,#26990,#26991),.UNSPECIFIED.,.F.,.F.)
B_SPLINE_CURVE_WITH_KNOTS((3,3),(2.065028853533E-6,0.0443073288439286),
 .UNSPECIFIED.)
CURVE()
GEOMETRIC_REPRESENTATION_ITEM()
RATIONAL_B_SPLINE_CURVE((1.00000000159591,1.00001712140699,1.00002048940404))
REPRESENTATION_ITEM('')
);
#1269=(
BOUNDED_CURVE()
B_SPLINE_CURVE(2,(#26995,#26996,#26997),.UNSPECIFIED.,.F.,.F.)
B_SPLINE_CURVE_WITH_KNOTS((3,3),(0.0660091927117083,0.110314456526682),
 .UNSPECIFIED.)
CURVE()
GEOMETRIC_REPRESENTATION_ITEM()
RATIONAL_B_SPLINE_CURVE((1.00002048940433,1.00001712140723,1.00000000159591))
REPRESENTATION_ITEM('')
);
#1270=(
BOUNDED_CURVE()
B_SPLINE_CURVE(2,(#27004,#27005,#27006),.UNSPECIFIED.,.F.,.F.)
B_SPLINE_CURVE_WITH_KNOTS((3,3),(7.86559624267222E-6,0.0612396373727971),
 .UNSPECIFIED.)
CURVE()
GEOMETRIC_REPRESENTATION_ITEM()
RATIONAL_B_SPLINE_CURVE((1.00001915745323,1.07458139657241,1.05821963517925))
REPRESENTATION_ITEM('')
);
#1271=(
BOUNDED_CURVE()
B_SPLINE_CURVE(2,(#27011,#27012,#27013),.UNSPECIFIED.,.F.,.F.)
B_SPLINE_CURVE_WITH_KNOTS((3,3),(0.0392023395450862,0.100434111321654),
 .UNSPECIFIED.)
CURVE()
GEOMETRIC_REPRESENTATION_ITEM()
RATIONAL_B_SPLINE_CURVE((1.05821963517913,1.07458139657226,1.0000191574532))
REPRESENTATION_ITEM('')
);
#1272=(
BOUNDED_CURVE()
B_SPLINE_CURVE(2,(#27029,#27030,#27031),.UNSPECIFIED.,.F.,.F.)
B_SPLINE_CURVE_WITH_KNOTS((3,3),(0.0142112171255263,0.110567648737579),
 .UNSPECIFIED.)
CURVE()
GEOMETRIC_REPRESENTATION_ITEM()
RATIONAL_B_SPLINE_CURVE((1.00000961768216,1.00003742652363,1.00000019074349))
REPRESENTATION_ITEM('')
);
#1273=(
BOUNDED_CURVE()
B_SPLINE_CURVE(2,(#27048,#27049,#27050),.UNSPECIFIED.,.F.,.F.)
B_SPLINE_CURVE_WITH_KNOTS((3,3),(0.000246247416178109,0.0445514940289694),
 .UNSPECIFIED.)
CURVE()
GEOMETRIC_REPRESENTATION_ITEM()
RATIONAL_B_SPLINE_CURVE((1.0000001907434,1.00001731196283,1.00002068136548))
REPRESENTATION_ITEM('')
);
#1274=(
BOUNDED_CURVE()
B_SPLINE_CURVE(2,(#27060,#27061,#27062),.UNSPECIFIED.,.F.,.F.)
B_SPLINE_CURVE_WITH_KNOTS((3,3),(0.000246247416177958,0.0966026790273509),
 .UNSPECIFIED.)
CURVE()
GEOMETRIC_REPRESENTATION_ITEM()
RATIONAL_B_SPLINE_CURVE((1.00000019074342,1.00003742650884,1.00000961767836))
REPRESENTATION_ITEM('')
);
#1275=(
BOUNDED_CURVE()
B_SPLINE_CURVE(2,(#27068,#27069,#27070),.UNSPECIFIED.,.F.,.F.)
B_SPLINE_CURVE_WITH_KNOTS((3,3),(0.0662624021247137,0.110567648737539),
 .UNSPECIFIED.)
CURVE()
GEOMETRIC_REPRESENTATION_ITEM()
RATIONAL_B_SPLINE_CURVE((1.00002068136864,1.00001731196548,1.00000019074343))
REPRESENTATION_ITEM('')
);
#1276=(
BOUNDED_CURVE()
B_SPLINE_CURVE(2,(#27088,#27089,#27090),.UNSPECIFIED.,.F.,.F.)
B_SPLINE_CURVE_WITH_KNOTS((3,3),(7.86559624408066E-6,0.0612396373727953),
 .UNSPECIFIED.)
CURVE()
GEOMETRIC_REPRESENTATION_ITEM()
RATIONAL_B_SPLINE_CURVE((1.00001915745323,1.07458139657215,1.05821963517905))
REPRESENTATION_ITEM('')
);
#1277=(
BOUNDED_CURVE()
B_SPLINE_CURVE(2,(#27098,#27099,#27100),.UNSPECIFIED.,.F.,.F.)
B_SPLINE_CURVE_WITH_KNOTS((3,3),(2.06499351984749E-6,0.0443065724919119),
 .UNSPECIFIED.)
CURVE()
GEOMETRIC_REPRESENTATION_ITEM()
RATIONAL_B_SPLINE_CURVE((1.00000000159957,1.00001716071212,1.00002056801068))
REPRESENTATION_ITEM('')
);
#1278=(
BOUNDED_CURVE()
B_SPLINE_CURVE(2,(#27102,#27103,#27104),.UNSPECIFIED.,.F.,.F.)
B_SPLINE_CURVE_WITH_KNOTS((3,3),(0.039202339545086,0.100434111321651),
 .UNSPECIFIED.)
CURVE()
GEOMETRIC_REPRESENTATION_ITEM()
RATIONAL_B_SPLINE_CURVE((1.05821963517915,1.0745813965723,1.00001915745321))
REPRESENTATION_ITEM('')
);
#1279=(
BOUNDED_CURVE()
B_SPLINE_CURVE(2,(#27110,#27111,#27112),.UNSPECIFIED.,.F.,.F.)
B_SPLINE_CURVE_WITH_KNOTS((3,3),(0.0142112171256635,0.110567648737569),
 .UNSPECIFIED.)
CURVE()
GEOMETRIC_REPRESENTATION_ITEM()
RATIONAL_B_SPLINE_CURVE((1.00000961767905,1.00003742651155,1.00000019074343))
REPRESENTATION_ITEM('')
);
#1280=(
BOUNDED_CURVE()
B_SPLINE_CURVE(2,(#27182,#27183,#27184),.UNSPECIFIED.,.F.,.F.)
B_SPLINE_CURVE_WITH_KNOTS((3,3),(0.0662606539244983,0.110565163369973),
 .UNSPECIFIED.)
CURVE()
GEOMETRIC_REPRESENTATION_ITEM()
RATIONAL_B_SPLINE_CURVE((1.00002056781132,1.00001716061344,1.00000000159956))
REPRESENTATION_ITEM('')
);
#1281=(
BOUNDED_CURVE()
B_SPLINE_CURVE(2,(#27191,#27192,#27193),.UNSPECIFIED.,.F.,.F.)
B_SPLINE_CURVE_WITH_KNOTS((3,3),(7.86559624013797E-6,0.0612396373727866),
 .UNSPECIFIED.)
CURVE()
GEOMETRIC_REPRESENTATION_ITEM()
RATIONAL_B_SPLINE_CURVE((1.00001915745322,1.07458139657224,1.05821963517911))
REPRESENTATION_ITEM('')
);
#1282=(
BOUNDED_CURVE()
B_SPLINE_CURVE(2,(#27198,#27199,#27200),.UNSPECIFIED.,.F.,.F.)
B_SPLINE_CURVE_WITH_KNOTS((3,3),(0.0392023395450931,0.100434111321664),
 .UNSPECIFIED.)
CURVE()
GEOMETRIC_REPRESENTATION_ITEM()
RATIONAL_B_SPLINE_CURVE((1.05821963517915,1.07458139657229,1.0000191574532))
REPRESENTATION_ITEM('')
);
#1283=(
BOUNDED_CURVE()
B_SPLINE_CURVE(2,(#27218,#27219,#27220),.UNSPECIFIED.,.F.,.F.)
B_SPLINE_CURVE_WITH_KNOTS((3,3),(2.06502885237961E-6,0.0443073288438955),
 .UNSPECIFIED.)
CURVE()
GEOMETRIC_REPRESENTATION_ITEM()
RATIONAL_B_SPLINE_CURVE((1.00000000159591,1.00001712140489,1.00002048940153))
REPRESENTATION_ITEM('')
);
#1284=(
BOUNDED_CURVE()
B_SPLINE_CURVE(2,(#27224,#27225,#27226),.UNSPECIFIED.,.F.,.F.)
B_SPLINE_CURVE_WITH_KNOTS((3,3),(0.0660091927116133,0.110314456526713),
 .UNSPECIFIED.)
CURVE()
GEOMETRIC_REPRESENTATION_ITEM()
RATIONAL_B_SPLINE_CURVE((1.00002048940597,1.0000171214086,1.00000000159591))
REPRESENTATION_ITEM('')
);
#1285=(
BOUNDED_CURVE()
B_SPLINE_CURVE(2,(#27233,#27234,#27235),.UNSPECIFIED.,.F.,.F.)
B_SPLINE_CURVE_WITH_KNOTS((3,3),(7.86559624719566E-6,0.0612396373727914),
 .UNSPECIFIED.)
CURVE()
GEOMETRIC_REPRESENTATION_ITEM()
RATIONAL_B_SPLINE_CURVE((1.00001915745324,1.07458139657227,1.05821963517913))
REPRESENTATION_ITEM('')
);
#1286=(
BOUNDED_CURVE()
B_SPLINE_CURVE(2,(#27240,#27241,#27242),.UNSPECIFIED.,.F.,.F.)
B_SPLINE_CURVE_WITH_KNOTS((3,3),(0.0392023395450766,0.100434111321633),
 .UNSPECIFIED.)
CURVE()
GEOMETRIC_REPRESENTATION_ITEM()
RATIONAL_B_SPLINE_CURVE((1.05821963517913,1.07458139657227,1.0000191574532))
REPRESENTATION_ITEM('')
);
#1287=(
BOUNDED_CURVE()
B_SPLINE_CURVE(2,(#27260,#27261,#27262),.UNSPECIFIED.,.F.,.F.)
B_SPLINE_CURVE_WITH_KNOTS((3,3),(2.0650288492734E-6,0.0443073288439416),
 .UNSPECIFIED.)
CURVE()
GEOMETRIC_REPRESENTATION_ITEM()
RATIONAL_B_SPLINE_CURVE((1.00000000159591,1.00001712140949,1.00002048940704))
REPRESENTATION_ITEM('')
);
#1288=(
BOUNDED_CURVE()
B_SPLINE_CURVE(2,(#27266,#27267,#27268),.UNSPECIFIED.,.F.,.F.)
B_SPLINE_CURVE_WITH_KNOTS((3,3),(0.06600919271168,0.110314456526681),
 .UNSPECIFIED.)
CURVE()
GEOMETRIC_REPRESENTATION_ITEM()
RATIONAL_B_SPLINE_CURVE((1.00002048940869,1.00001712141088,1.00000000159591))
REPRESENTATION_ITEM('')
);
#1289=(
BOUNDED_CURVE()
B_SPLINE_CURVE(2,(#27275,#27276,#27277),.UNSPECIFIED.,.F.,.F.)
B_SPLINE_CURVE_WITH_KNOTS((3,3),(7.86559623979792E-6,0.0612396373727948),
 .UNSPECIFIED.)
CURVE()
GEOMETRIC_REPRESENTATION_ITEM()
RATIONAL_B_SPLINE_CURVE((1.00001915745322,1.0745813965724,1.05821963517924))
REPRESENTATION_ITEM('')
);
#1290=(
BOUNDED_CURVE()
B_SPLINE_CURVE(2,(#27282,#27283,#27284),.UNSPECIFIED.,.F.,.F.)
B_SPLINE_CURVE_WITH_KNOTS((3,3),(0.0392023395450884,0.100434111321653),
 .UNSPECIFIED.)
CURVE()
GEOMETRIC_REPRESENTATION_ITEM()
RATIONAL_B_SPLINE_CURVE((1.05821963517909,1.07458139657222,1.00001915745319))
REPRESENTATION_ITEM('')
);
#1291=(
BOUNDED_CURVE()
B_SPLINE_CURVE(2,(#27302,#27303,#27304),.UNSPECIFIED.,.F.,.F.)
B_SPLINE_CURVE_WITH_KNOTS((3,3),(2.06502884853687E-6,0.0443073288438766),
 .UNSPECIFIED.)
CURVE()
GEOMETRIC_REPRESENTATION_ITEM()
RATIONAL_B_SPLINE_CURVE((1.00000000159591,1.00001712141175,1.00002048940974))
REPRESENTATION_ITEM('')
);
#1292=(
BOUNDED_CURVE()
B_SPLINE_CURVE(2,(#27308,#27309,#27310),.UNSPECIFIED.,.F.,.F.)
B_SPLINE_CURVE_WITH_KNOTS((3,3),(0.0660091927116071,0.110314456526712),
 .UNSPECIFIED.)
CURVE()
GEOMETRIC_REPRESENTATION_ITEM()
RATIONAL_B_SPLINE_CURVE((1.00002048940052,1.00001712140405,1.00000000159591))
REPRESENTATION_ITEM('')
);
#1293=(
BOUNDED_CURVE()
B_SPLINE_CURVE(2,(#27317,#27318,#27319),.UNSPECIFIED.,.F.,.F.)
B_SPLINE_CURVE_WITH_KNOTS((3,3),(7.86559623158078E-6,0.0612396373727783),
 .UNSPECIFIED.)
CURVE()
GEOMETRIC_REPRESENTATION_ITEM()
RATIONAL_B_SPLINE_CURVE((1.0000191574532,1.07458139657216,1.05821963517905))
REPRESENTATION_ITEM('')
);
#1294=(
BOUNDED_CURVE()
B_SPLINE_CURVE(2,(#27324,#27325,#27326),.UNSPECIFIED.,.F.,.F.)
B_SPLINE_CURVE_WITH_KNOTS((3,3),(0.039202339545081,0.100434111321637),
 .UNSPECIFIED.)
CURVE()
GEOMETRIC_REPRESENTATION_ITEM()
RATIONAL_B_SPLINE_CURVE((1.05821963517899,1.07458139657208,1.00001915745317))
REPRESENTATION_ITEM('')
);
#1295=(
BOUNDED_CURVE()
B_SPLINE_CURVE(2,(#27344,#27345,#27346),.UNSPECIFIED.,.F.,.F.)
B_SPLINE_CURVE_WITH_KNOTS((3,3),(2.06502885037694E-6,0.0443073288438504),
 .UNSPECIFIED.)
CURVE()
GEOMETRIC_REPRESENTATION_ITEM()
RATIONAL_B_SPLINE_CURVE((1.00000000159591,1.00001712141043,1.00002048940816))
REPRESENTATION_ITEM('')
);
#1296=(
BOUNDED_CURVE()
B_SPLINE_CURVE(2,(#27350,#27351,#27352),.UNSPECIFIED.,.F.,.F.)
B_SPLINE_CURVE_WITH_KNOTS((3,3),(0.0660091927116714,0.110314456526714),
 .UNSPECIFIED.)
CURVE()
GEOMETRIC_REPRESENTATION_ITEM()
RATIONAL_B_SPLINE_CURVE((1.00002048940854,1.00001712141075,1.00000000159591))
REPRESENTATION_ITEM('')
);
#1297=(
BOUNDED_CURVE()
B_SPLINE_CURVE(2,(#27359,#27360,#27361),.UNSPECIFIED.,.F.,.F.)
B_SPLINE_CURVE_WITH_KNOTS((3,3),(7.86559624227606E-6,0.0612396373727856),
 .UNSPECIFIED.)
CURVE()
GEOMETRIC_REPRESENTATION_ITEM()
RATIONAL_B_SPLINE_CURVE((1.00001915745323,1.07458139657213,1.05821963517903))
REPRESENTATION_ITEM('')
);
#1298=(
BOUNDED_CURVE()
B_SPLINE_CURVE(2,(#27366,#27367,#27368),.UNSPECIFIED.,.F.,.F.)
B_SPLINE_CURVE_WITH_KNOTS((3,3),(0.0392023395450793,0.100434111321634),
 .UNSPECIFIED.)
CURVE()
GEOMETRIC_REPRESENTATION_ITEM()
RATIONAL_B_SPLINE_CURVE((1.0582196351791,1.07458139657223,1.00001915745319))
REPRESENTATION_ITEM('')
);
#1299=(
BOUNDED_CURVE()
B_SPLINE_CURVE(2,(#27386,#27387,#27388),.UNSPECIFIED.,.F.,.F.)
B_SPLINE_CURVE_WITH_KNOTS((3,3),(2.06502885144773E-6,0.044307328843974),
 .UNSPECIFIED.)
CURVE()
GEOMETRIC_REPRESENTATION_ITEM()
RATIONAL_B_SPLINE_CURVE((1.00000000159591,1.00001712140841,1.00002048940574))
REPRESENTATION_ITEM('')
);
#1300=(
BOUNDED_CURVE()
B_SPLINE_CURVE(2,(#27392,#27393,#27394),.UNSPECIFIED.,.F.,.F.)
B_SPLINE_CURVE_WITH_KNOTS((3,3),(0.0660091927116272,0.110314456526716),
 .UNSPECIFIED.)
CURVE()
GEOMETRIC_REPRESENTATION_ITEM()
RATIONAL_B_SPLINE_CURVE((1.00002048940471,1.00001712140755,1.00000000159591))
REPRESENTATION_ITEM('')
);
#1301=(
BOUNDED_CURVE()
B_SPLINE_CURVE(2,(#27401,#27402,#27403),.UNSPECIFIED.,.F.,.F.)
B_SPLINE_CURVE_WITH_KNOTS((3,3),(7.86559623316717E-6,0.0612396373727784),
 .UNSPECIFIED.)
CURVE()
GEOMETRIC_REPRESENTATION_ITEM()
RATIONAL_B_SPLINE_CURVE((1.0000191574532,1.07458139657221,1.05821963517909))
REPRESENTATION_ITEM('')
);
#1302=(
BOUNDED_CURVE()
B_SPLINE_CURVE(2,(#27408,#27409,#27410),.UNSPECIFIED.,.F.,.F.)
B_SPLINE_CURVE_WITH_KNOTS((3,3),(0.0392023395450884,0.100434111321648),
 .UNSPECIFIED.)
CURVE()
GEOMETRIC_REPRESENTATION_ITEM()
RATIONAL_B_SPLINE_CURVE((1.05821963517895,1.07458139657204,1.00001915745322))
REPRESENTATION_ITEM('')
);
#1303=(
BOUNDED_CURVE()
B_SPLINE_CURVE(2,(#27428,#27429,#27430),.UNSPECIFIED.,.F.,.F.)
B_SPLINE_CURVE_WITH_KNOTS((3,3),(2.06502884894631E-6,0.0443073288438279),
 .UNSPECIFIED.)
CURVE()
GEOMETRIC_REPRESENTATION_ITEM()
RATIONAL_B_SPLINE_CURVE((1.00000000159591,1.00001712141452,1.00002048941305))
REPRESENTATION_ITEM('')
);
#1304=(
BOUNDED_CURVE()
B_SPLINE_CURVE(2,(#27434,#27435,#27436),.UNSPECIFIED.,.F.,.F.)
B_SPLINE_CURVE_WITH_KNOTS((3,3),(0.0660091927115484,0.110314456526686),
 .UNSPECIFIED.)
CURVE()
GEOMETRIC_REPRESENTATION_ITEM()
RATIONAL_B_SPLINE_CURVE((1.00002048939942,1.00001712140313,1.00000000159591))
REPRESENTATION_ITEM('')
);
#1305=(
BOUNDED_CURVE()
B_SPLINE_CURVE(2,(#27443,#27444,#27445),.UNSPECIFIED.,.F.,.F.)
B_SPLINE_CURVE_WITH_KNOTS((3,3),(7.86559624503439E-6,0.0612396373727955),
 .UNSPECIFIED.)
CURVE()
GEOMETRIC_REPRESENTATION_ITEM()
RATIONAL_B_SPLINE_CURVE((1.00001915745323,1.07458139657222,1.0582196351791))
REPRESENTATION_ITEM('')
);
#1306=(
BOUNDED_CURVE()
B_SPLINE_CURVE(2,(#27450,#27451,#27452),.UNSPECIFIED.,.F.,.F.)
B_SPLINE_CURVE_WITH_KNOTS((3,3),(0.0392023395450828,0.100434111321649),
 .UNSPECIFIED.)
CURVE()
GEOMETRIC_REPRESENTATION_ITEM()
RATIONAL_B_SPLINE_CURVE((1.05821963517927,1.07458139657245,1.00001915745322))
REPRESENTATION_ITEM('')
);
#1307=(
BOUNDED_CURVE()
B_SPLINE_CURVE(2,(#27470,#27471,#27472),.UNSPECIFIED.,.F.,.F.)
B_SPLINE_CURVE_WITH_KNOTS((3,3),(2.06502884806617E-6,0.044307328843884),
 .UNSPECIFIED.)
CURVE()
GEOMETRIC_REPRESENTATION_ITEM()
RATIONAL_B_SPLINE_CURVE((1.00000000159591,1.00001712140915,1.00002048940663))
REPRESENTATION_ITEM('')
);
#1308=(
BOUNDED_CURVE()
B_SPLINE_CURVE(2,(#27476,#27477,#27478),.UNSPECIFIED.,.F.,.F.)
B_SPLINE_CURVE_WITH_KNOTS((3,3),(0.0660091927117217,0.110314456526714),
 .UNSPECIFIED.)
CURVE()
GEOMETRIC_REPRESENTATION_ITEM()
RATIONAL_B_SPLINE_CURVE((1.00002048940948,1.00001712141153,1.00000000159591))
REPRESENTATION_ITEM('')
);
#1309=(
BOUNDED_CURVE()
B_SPLINE_CURVE(2,(#27485,#27486,#27487),.UNSPECIFIED.,.F.,.F.)
B_SPLINE_CURVE_WITH_KNOTS((3,3),(7.86559623218909E-6,0.0612396373727783),
 .UNSPECIFIED.)
CURVE()
GEOMETRIC_REPRESENTATION_ITEM()
RATIONAL_B_SPLINE_CURVE((1.0000191574532,1.07458139657225,1.05821963517912))
REPRESENTATION_ITEM('')
);
#1310=(
BOUNDED_CURVE()
B_SPLINE_CURVE(2,(#27492,#27493,#27494),.UNSPECIFIED.,.F.,.F.)
B_SPLINE_CURVE_WITH_KNOTS((3,3),(0.0392023395450802,0.100434111321634),
 .UNSPECIFIED.)
CURVE()
GEOMETRIC_REPRESENTATION_ITEM()
RATIONAL_B_SPLINE_CURVE((1.05821963517902,1.07458139657212,1.0000191574532))
REPRESENTATION_ITEM('')
);
#1311=(
BOUNDED_CURVE()
B_SPLINE_CURVE(2,(#27510,#27511,#27512),.UNSPECIFIED.,.F.,.F.)
B_SPLINE_CURVE_WITH_KNOTS((3,3),(0.0142112171256889,0.110567648737577),
 .UNSPECIFIED.)
CURVE()
GEOMETRIC_REPRESENTATION_ITEM()
RATIONAL_B_SPLINE_CURVE((1.00000961767866,1.00003742651004,1.00000019074342))
REPRESENTATION_ITEM('')
);
#1312=(
BOUNDED_CURVE()
B_SPLINE_CURVE(2,(#27529,#27530,#27531),.UNSPECIFIED.,.F.,.F.)
B_SPLINE_CURVE_WITH_KNOTS((3,3),(0.000246247416171589,0.0445514940288941),
 .UNSPECIFIED.)
CURVE()
GEOMETRIC_REPRESENTATION_ITEM()
RATIONAL_B_SPLINE_CURVE((1.00000019074345,1.00001731196734,1.00002068137086))
REPRESENTATION_ITEM('')
);
#1313=(
BOUNDED_CURVE()
B_SPLINE_CURVE(2,(#27541,#27542,#27543),.UNSPECIFIED.,.F.,.F.)
B_SPLINE_CURVE_WITH_KNOTS((3,3),(0.000246247416178378,0.0966026790274705),
 .UNSPECIFIED.)
CURVE()
GEOMETRIC_REPRESENTATION_ITEM()
RATIONAL_B_SPLINE_CURVE((1.00000019074344,1.00003742651365,1.00000961767959))
REPRESENTATION_ITEM('')
);
#1314=(
BOUNDED_CURVE()
B_SPLINE_CURVE(2,(#27549,#27550,#27551),.UNSPECIFIED.,.F.,.F.)
B_SPLINE_CURVE_WITH_KNOTS((3,3),(0.0142112171255851,0.11056764873757),
 .UNSPECIFIED.)
CURVE()
GEOMETRIC_REPRESENTATION_ITEM()
RATIONAL_B_SPLINE_CURVE((1.00000961768111,1.00003742651954,1.00000019074347))
REPRESENTATION_ITEM('')
);
#1315=(
BOUNDED_CURVE()
B_SPLINE_CURVE(2,(#27624,#27625,#27626),.UNSPECIFIED.,.F.,.F.)
B_SPLINE_CURVE_WITH_KNOTS((3,3),(0.000496318296887013,0.0448015472108987),
 .UNSPECIFIED.)
CURVE()
GEOMETRIC_REPRESENTATION_ITEM()
RATIONAL_B_SPLINE_CURVE((1.00000038535058,1.00001750801892,1.00002087886772))
REPRESENTATION_ITEM('')
);
#1316=(
BOUNDED_CURVE()
B_SPLINE_CURVE(2,(#27632,#27633,#27634),.UNSPECIFIED.,.F.,.F.)
B_SPLINE_CURVE_WITH_KNOTS((3,3),(0.0665217606070769,0.110826989520968),
 .UNSPECIFIED.)
CURVE()
GEOMETRIC_REPRESENTATION_ITEM()
RATIONAL_B_SPLINE_CURVE((1.0000208788742,1.00001750802436,1.0000003853507))
REPRESENTATION_ITEM('')
);
#1317=(
BOUNDED_CURVE()
B_SPLINE_CURVE(2,(#27648,#27649,#27650),.UNSPECIFIED.,.F.,.F.)
B_SPLINE_CURVE_WITH_KNOTS((3,3),(7.86559624534712E-6,0.061239637372799),
 .UNSPECIFIED.)
CURVE()
GEOMETRIC_REPRESENTATION_ITEM()
RATIONAL_B_SPLINE_CURVE((1.00001915745323,1.07458139657233,1.05821963517918))
REPRESENTATION_ITEM('')
);
#1318=(
BOUNDED_CURVE()
B_SPLINE_CURVE(2,(#27658,#27659,#27660),.UNSPECIFIED.,.F.,.F.)
B_SPLINE_CURVE_WITH_KNOTS((3,3),(2.06502884745806E-6,0.0443073288438634),
 .UNSPECIFIED.)
CURVE()
GEOMETRIC_REPRESENTATION_ITEM()
RATIONAL_B_SPLINE_CURVE((1.00000000159591,1.00001712141092,1.00002048940875))
REPRESENTATION_ITEM('')
);
#1319=(
BOUNDED_CURVE()
B_SPLINE_CURVE(2,(#27662,#27663,#27664),.UNSPECIFIED.,.F.,.F.)
B_SPLINE_CURVE_WITH_KNOTS((3,3),(0.0392023395450795,0.100434111321635),
 .UNSPECIFIED.)
CURVE()
GEOMETRIC_REPRESENTATION_ITEM()
RATIONAL_B_SPLINE_CURVE((1.05821963517901,1.07458139657211,1.00001915745319))
REPRESENTATION_ITEM('')
);
#1320=(
BOUNDED_CURVE()
B_SPLINE_CURVE(2,(#27670,#27671,#27672),.UNSPECIFIED.,.F.,.F.)
B_SPLINE_CURVE_WITH_KNOTS((3,3),(0.0660091927116517,0.110314456526715),
 .UNSPECIFIED.)
CURVE()
GEOMETRIC_REPRESENTATION_ITEM()
RATIONAL_B_SPLINE_CURVE((1.00002048940891,1.00001712141106,1.00000000159591))
REPRESENTATION_ITEM('')
);
#1321=(
BOUNDED_CURVE()
B_SPLINE_CURVE(2,(#27690,#27691,#27692),.UNSPECIFIED.,.F.,.F.)
B_SPLINE_CURVE_WITH_KNOTS((3,3),(7.86559623604086E-6,0.0612396373727819),
 .UNSPECIFIED.)
CURVE()
GEOMETRIC_REPRESENTATION_ITEM()
RATIONAL_B_SPLINE_CURVE((1.00001915745321,1.07458139657227,1.05821963517914))
REPRESENTATION_ITEM('')
);
#1322=(
BOUNDED_CURVE()
B_SPLINE_CURVE(2,(#27700,#27701,#27702),.UNSPECIFIED.,.F.,.F.)
B_SPLINE_CURVE_WITH_KNOTS((3,3),(2.06502884700055E-6,0.0443073288438819),
 .UNSPECIFIED.)
CURVE()
GEOMETRIC_REPRESENTATION_ITEM()
RATIONAL_B_SPLINE_CURVE((1.00000000159591,1.00001712140918,1.00002048940666))
REPRESENTATION_ITEM('')
);
#1323=(
BOUNDED_CURVE()
B_SPLINE_CURVE(2,(#27704,#27705,#27706),.UNSPECIFIED.,.F.,.F.)
B_SPLINE_CURVE_WITH_KNOTS((3,3),(0.0392023395450774,0.100434111321637),
 .UNSPECIFIED.)
CURVE()
GEOMETRIC_REPRESENTATION_ITEM()
RATIONAL_B_SPLINE_CURVE((1.05821963517918,1.07458139657232,1.00001915745317))
REPRESENTATION_ITEM('')
);
#1324=(
BOUNDED_CURVE()
B_SPLINE_CURVE(2,(#27712,#27713,#27714),.UNSPECIFIED.,.F.,.F.)
B_SPLINE_CURVE_WITH_KNOTS((3,3),(0.0660091927116316,0.110314456526682),
 .UNSPECIFIED.)
CURVE()
GEOMETRIC_REPRESENTATION_ITEM()
RATIONAL_B_SPLINE_CURVE((1.00002048940402,1.00001712140697,1.00000000159591))
REPRESENTATION_ITEM('')
);
#1325=(
BOUNDED_CURVE()
B_SPLINE_CURVE(2,(#27732,#27733,#27734),.UNSPECIFIED.,.F.,.F.)
B_SPLINE_CURVE_WITH_KNOTS((3,3),(7.86559623940256E-6,0.0612396373727946),
 .UNSPECIFIED.)
CURVE()
GEOMETRIC_REPRESENTATION_ITEM()
RATIONAL_B_SPLINE_CURVE((1.00001915745322,1.0745813965724,1.05821963517923))
REPRESENTATION_ITEM('')
);
#1326=(
BOUNDED_CURVE()
B_SPLINE_CURVE(2,(#27742,#27743,#27744),.UNSPECIFIED.,.F.,.F.)
B_SPLINE_CURVE_WITH_KNOTS((3,3),(2.06502884915366E-6,0.0443073288438936),
 .UNSPECIFIED.)
CURVE()
GEOMETRIC_REPRESENTATION_ITEM()
RATIONAL_B_SPLINE_CURVE((1.00000000159591,1.00001712141024,1.00002048940794))
REPRESENTATION_ITEM('')
);
#1327=(
BOUNDED_CURVE()
B_SPLINE_CURVE(2,(#27746,#27747,#27748),.UNSPECIFIED.,.F.,.F.)
B_SPLINE_CURVE_WITH_KNOTS((3,3),(0.0392023395450764,0.100434111321633),
 .UNSPECIFIED.)
CURVE()
GEOMETRIC_REPRESENTATION_ITEM()
RATIONAL_B_SPLINE_CURVE((1.05821963517915,1.07458139657229,1.00001915745319))
REPRESENTATION_ITEM('')
);
#1328=(
BOUNDED_CURVE()
B_SPLINE_CURVE(2,(#27754,#27755,#27756),.UNSPECIFIED.,.F.,.F.)
B_SPLINE_CURVE_WITH_KNOTS((3,3),(0.0660091927116924,0.110314456526717),
 .UNSPECIFIED.)
CURVE()
GEOMETRIC_REPRESENTATION_ITEM()
RATIONAL_B_SPLINE_CURVE((1.00002048940367,1.00001712140668,1.00000000159591))
REPRESENTATION_ITEM('')
);
#1329=(
BOUNDED_CURVE()
B_SPLINE_CURVE(2,(#27774,#27775,#27776),.UNSPECIFIED.,.F.,.F.)
B_SPLINE_CURVE_WITH_KNOTS((3,3),(7.86559623680102E-6,0.0612396373727785),
 .UNSPECIFIED.)
CURVE()
GEOMETRIC_REPRESENTATION_ITEM()
RATIONAL_B_SPLINE_CURVE((1.00001915745321,1.074581396572,1.05821963517893))
REPRESENTATION_ITEM('')
);
#1330=(
BOUNDED_CURVE()
B_SPLINE_CURVE(2,(#27784,#27785,#27786),.UNSPECIFIED.,.F.,.F.)
B_SPLINE_CURVE_WITH_KNOTS((3,3),(2.06502885214286E-6,0.0443073288438507),
 .UNSPECIFIED.)
CURVE()
GEOMETRIC_REPRESENTATION_ITEM()
RATIONAL_B_SPLINE_CURVE((1.00000000159591,1.00001712141213,1.0000204894102))
REPRESENTATION_ITEM('')
);
#1331=(
BOUNDED_CURVE()
B_SPLINE_CURVE(2,(#27788,#27789,#27790),.UNSPECIFIED.,.F.,.F.)
B_SPLINE_CURVE_WITH_KNOTS((3,3),(0.0392023395450757,0.100434111321633),
 .UNSPECIFIED.)
CURVE()
GEOMETRIC_REPRESENTATION_ITEM()
RATIONAL_B_SPLINE_CURVE((1.05821963517913,1.07458139657228,1.0000191574532))
REPRESENTATION_ITEM('')
);
#1332=(
BOUNDED_CURVE()
B_SPLINE_CURVE(2,(#27796,#27797,#27798),.UNSPECIFIED.,.F.,.F.)
B_SPLINE_CURVE_WITH_KNOTS((3,3),(0.0660091927116415,0.110314456526713),
 .UNSPECIFIED.)
CURVE()
GEOMETRIC_REPRESENTATION_ITEM()
RATIONAL_B_SPLINE_CURVE((1.00002048940584,1.00001712140849,1.00000000159591))
REPRESENTATION_ITEM('')
);
#1333=(
BOUNDED_CURVE()
B_SPLINE_CURVE(2,(#27816,#27817,#27818),.UNSPECIFIED.,.F.,.F.)
B_SPLINE_CURVE_WITH_KNOTS((3,3),(7.86559624497379E-6,0.0612396373727874),
 .UNSPECIFIED.)
CURVE()
GEOMETRIC_REPRESENTATION_ITEM()
RATIONAL_B_SPLINE_CURVE((1.00001915745323,1.07458139657225,1.05821963517912))
REPRESENTATION_ITEM('')
);
#1334=(
BOUNDED_CURVE()
B_SPLINE_CURVE(2,(#27826,#27827,#27828),.UNSPECIFIED.,.F.,.F.)
B_SPLINE_CURVE_WITH_KNOTS((3,3),(2.06502884959385E-6,0.0443073288439219),
 .UNSPECIFIED.)
CURVE()
GEOMETRIC_REPRESENTATION_ITEM()
RATIONAL_B_SPLINE_CURVE((1.00000000159591,1.00001712140764,1.00002048940482))
REPRESENTATION_ITEM('')
);
#1335=(
BOUNDED_CURVE()
B_SPLINE_CURVE(2,(#27830,#27831,#27832),.UNSPECIFIED.,.F.,.F.)
B_SPLINE_CURVE_WITH_KNOTS((3,3),(0.0392023395450757,0.100434111321633),
 .UNSPECIFIED.)
CURVE()
GEOMETRIC_REPRESENTATION_ITEM()
RATIONAL_B_SPLINE_CURVE((1.05821963517915,1.0745813965723,1.00001915745321))
REPRESENTATION_ITEM('')
);
#1336=(
BOUNDED_CURVE()
B_SPLINE_CURVE(2,(#27838,#27839,#27840),.UNSPECIFIED.,.F.,.F.)
B_SPLINE_CURVE_WITH_KNOTS((3,3),(0.0660091927117066,0.110314456526683),
 .UNSPECIFIED.)
CURVE()
GEOMETRIC_REPRESENTATION_ITEM()
RATIONAL_B_SPLINE_CURVE((1.00002048940495,1.00001712140775,1.00000000159591))
REPRESENTATION_ITEM('')
);
#1337=(
BOUNDED_CURVE()
B_SPLINE_CURVE(2,(#27858,#27859,#27860),.UNSPECIFIED.,.F.,.F.)
B_SPLINE_CURVE_WITH_KNOTS((3,3),(7.86559625117044E-6,0.0612396373728031),
 .UNSPECIFIED.)
CURVE()
GEOMETRIC_REPRESENTATION_ITEM()
RATIONAL_B_SPLINE_CURVE((1.00001915745325,1.07458139657221,1.05821963517909))
REPRESENTATION_ITEM('')
);
#1338=(
BOUNDED_CURVE()
B_SPLINE_CURVE(2,(#27868,#27869,#27870),.UNSPECIFIED.,.F.,.F.)
B_SPLINE_CURVE_WITH_KNOTS((3,3),(2.06502885431328E-6,0.0443073288438909),
 .UNSPECIFIED.)
CURVE()
GEOMETRIC_REPRESENTATION_ITEM()
RATIONAL_B_SPLINE_CURVE((1.00000000159591,1.00001712140729,1.0000204894044))
REPRESENTATION_ITEM('')
);
#1339=(
BOUNDED_CURVE()
B_SPLINE_CURVE(2,(#27872,#27873,#27874),.UNSPECIFIED.,.F.,.F.)
B_SPLINE_CURVE_WITH_KNOTS((3,3),(0.0392023395450745,0.100434111321634),
 .UNSPECIFIED.)
CURVE()
GEOMETRIC_REPRESENTATION_ITEM()
RATIONAL_B_SPLINE_CURVE((1.05821963517924,1.07458139657242,1.00001915745323))
REPRESENTATION_ITEM('')
);
#1340=(
BOUNDED_CURVE()
B_SPLINE_CURVE(2,(#27880,#27881,#27882),.UNSPECIFIED.,.F.,.F.)
B_SPLINE_CURVE_WITH_KNOTS((3,3),(0.0660091927116867,0.110314456526718),
 .UNSPECIFIED.)
CURVE()
GEOMETRIC_REPRESENTATION_ITEM()
RATIONAL_B_SPLINE_CURVE((1.00002048940563,1.00001712140832,1.00000000159591))
REPRESENTATION_ITEM('')
);
#1341=(
BOUNDED_CURVE()
B_SPLINE_CURVE(2,(#27900,#27901,#27902),.UNSPECIFIED.,.F.,.F.)
B_SPLINE_CURVE_WITH_KNOTS((3,3),(7.86559624197589E-6,0.0612396373727868),
 .UNSPECIFIED.)
CURVE()
GEOMETRIC_REPRESENTATION_ITEM()
RATIONAL_B_SPLINE_CURVE((1.00001915745323,1.07458139657218,1.05821963517906))
REPRESENTATION_ITEM('')
);
#1342=(
BOUNDED_CURVE()
B_SPLINE_CURVE(2,(#27910,#27911,#27912),.UNSPECIFIED.,.F.,.F.)
B_SPLINE_CURVE_WITH_KNOTS((3,3),(2.06502884662093E-6,0.0443073288437533),
 .UNSPECIFIED.)
CURVE()
GEOMETRIC_REPRESENTATION_ITEM()
RATIONAL_B_SPLINE_CURVE((1.00000000159591,1.0000171214157,1.00002048941447))
REPRESENTATION_ITEM('')
);
#1343=(
BOUNDED_CURVE()
B_SPLINE_CURVE(2,(#27914,#27915,#27916),.UNSPECIFIED.,.F.,.F.)
B_SPLINE_CURVE_WITH_KNOTS((3,3),(0.0392023395450786,0.100434111321633),
 .UNSPECIFIED.)
CURVE()
GEOMETRIC_REPRESENTATION_ITEM()
RATIONAL_B_SPLINE_CURVE((1.05821963517905,1.07458139657217,1.00001915745321))
REPRESENTATION_ITEM('')
);
#1344=(
BOUNDED_CURVE()
B_SPLINE_CURVE(2,(#27922,#27923,#27924),.UNSPECIFIED.,.F.,.F.)
B_SPLINE_CURVE_WITH_KNOTS((3,3),(0.0660091927117032,0.110314456526714),
 .UNSPECIFIED.)
CURVE()
GEOMETRIC_REPRESENTATION_ITEM()
RATIONAL_B_SPLINE_CURVE((1.0000204894113,1.00001712141305,1.00000000159591))
REPRESENTATION_ITEM('')
);
#1345=(
BOUNDED_CURVE()
B_SPLINE_CURVE(2,(#27942,#27943,#27944),.UNSPECIFIED.,.F.,.F.)
B_SPLINE_CURVE_WITH_KNOTS((3,3),(7.86559625570308E-6,0.0612396373727984),
 .UNSPECIFIED.)
CURVE()
GEOMETRIC_REPRESENTATION_ITEM()
RATIONAL_B_SPLINE_CURVE((1.00001915745326,1.07458139657228,1.05821963517913))
REPRESENTATION_ITEM('')
);
#1346=(
BOUNDED_CURVE()
B_SPLINE_CURVE(2,(#27952,#27953,#27954),.UNSPECIFIED.,.F.,.F.)
B_SPLINE_CURVE_WITH_KNOTS((3,3),(2.06502885013862E-6,0.0443073288438289),
 .UNSPECIFIED.)
CURVE()
GEOMETRIC_REPRESENTATION_ITEM()
RATIONAL_B_SPLINE_CURVE((1.00000000159591,1.00001712141,1.00002048940764))
REPRESENTATION_ITEM('')
);
#1347=(
BOUNDED_CURVE()
B_SPLINE_CURVE(2,(#27956,#27957,#27958),.UNSPECIFIED.,.F.,.F.)
B_SPLINE_CURVE_WITH_KNOTS((3,3),(0.0392023395450752,0.100434111321631),
 .UNSPECIFIED.)
CURVE()
GEOMETRIC_REPRESENTATION_ITEM()
RATIONAL_B_SPLINE_CURVE((1.05821963517917,1.07458139657232,1.00001915745323))
REPRESENTATION_ITEM('')
);
#1348=(
BOUNDED_CURVE()
B_SPLINE_CURVE(2,(#27964,#27965,#27966),.UNSPECIFIED.,.F.,.F.)
B_SPLINE_CURVE_WITH_KNOTS((3,3),(0.0660091927116231,0.110314456526669),
 .UNSPECIFIED.)
CURVE()
GEOMETRIC_REPRESENTATION_ITEM()
RATIONAL_B_SPLINE_CURVE((1.00002048940694,1.00001712140941,1.00000000159591))
REPRESENTATION_ITEM('')
);
#1349=(
BOUNDED_CURVE()
B_SPLINE_CURVE(2,(#27983,#27984,#27985),.UNSPECIFIED.,.F.,.F.)
B_SPLINE_CURVE_WITH_KNOTS((3,3),(0.0392023395450754,0.100434111321632),
 .UNSPECIFIED.)
CURVE()
GEOMETRIC_REPRESENTATION_ITEM()
RATIONAL_B_SPLINE_CURVE((1.05821963517916,1.07458139657231,1.00001915745321))
REPRESENTATION_ITEM('')
);
#1350=(
BOUNDED_CURVE()
B_SPLINE_CURVE(2,(#27994,#27995,#27996),.UNSPECIFIED.,.F.,.F.)
B_SPLINE_CURVE_WITH_KNOTS((3,3),(7.86559624287504E-6,0.0612396373728),
 .UNSPECIFIED.)
CURVE()
GEOMETRIC_REPRESENTATION_ITEM()
RATIONAL_B_SPLINE_CURVE((1.00001915745323,1.07458139657225,1.05821963517912))
REPRESENTATION_ITEM('')
);
#1351=(
BOUNDED_CURVE()
B_SPLINE_CURVE(2,(#33696,#33697,#33698),.UNSPECIFIED.,.F.,.F.)
B_SPLINE_CURVE_WITH_KNOTS((3,3),(0.0914017655662012,0.12815983246024),
 .UNSPECIFIED.)
CURVE()
GEOMETRIC_REPRESENTATION_ITEM()
RATIONAL_B_SPLINE_CURVE((1.00900211770899,1.00952129238834,1.00900211770899))
REPRESENTATION_ITEM('')
);
#1352=(
BOUNDED_CURVE()
B_SPLINE_CURVE(2,(#33729,#33730,#33731),.UNSPECIFIED.,.F.,.F.)
B_SPLINE_CURVE_WITH_KNOTS((3,3),(0.091401765566201,0.12815983246024),
 .UNSPECIFIED.)
CURVE()
GEOMETRIC_REPRESENTATION_ITEM()
RATIONAL_B_SPLINE_CURVE((1.009002117709,1.00952129238836,1.009002117709))
REPRESENTATION_ITEM('')
);
#1353=(
BOUNDED_CURVE()
B_SPLINE_CURVE(2,(#33737,#33738,#33739),.UNSPECIFIED.,.F.,.F.)
B_SPLINE_CURVE_WITH_KNOTS((3,3),(0.0914017655662024,0.128159832460242),
 .UNSPECIFIED.)
CURVE()
GEOMETRIC_REPRESENTATION_ITEM()
RATIONAL_B_SPLINE_CURVE((1.00900211770901,1.00952129238837,1.00900211770901))
REPRESENTATION_ITEM('')
);
#1354=(
BOUNDED_CURVE()
B_SPLINE_CURVE(2,(#33770,#33771,#33772),.UNSPECIFIED.,.F.,.F.)
B_SPLINE_CURVE_WITH_KNOTS((3,3),(0.0914017655662023,0.128159832460241),
 .UNSPECIFIED.)
CURVE()
GEOMETRIC_REPRESENTATION_ITEM()
RATIONAL_B_SPLINE_CURVE((1.00900211770899,1.00952129238835,1.00900211770899))
REPRESENTATION_ITEM('')
);
#1355=(
BOUNDED_CURVE()
B_SPLINE_CURVE(2,(#33778,#33779,#33780),.UNSPECIFIED.,.F.,.F.)
B_SPLINE_CURVE_WITH_KNOTS((3,3),(0.091401765566202,0.128159832460241),
 .UNSPECIFIED.)
CURVE()
GEOMETRIC_REPRESENTATION_ITEM()
RATIONAL_B_SPLINE_CURVE((1.009002117709,1.00952129238836,1.009002117709))
REPRESENTATION_ITEM('')
);
#1356=(
BOUNDED_CURVE()
B_SPLINE_CURVE(2,(#33786,#33787,#33788),.UNSPECIFIED.,.F.,.F.)
B_SPLINE_CURVE_WITH_KNOTS((3,3),(0.0914017655662003,0.128159832460239),
 .UNSPECIFIED.)
CURVE()
GEOMETRIC_REPRESENTATION_ITEM()
RATIONAL_B_SPLINE_CURVE((1.009002117709,1.00952129238835,1.009002117709))
REPRESENTATION_ITEM('')
);
#1357=(
BOUNDED_CURVE()
B_SPLINE_CURVE(2,(#33792,#33793,#33794),.UNSPECIFIED.,.F.,.F.)
B_SPLINE_CURVE_WITH_KNOTS((3,3),(0.068123192861032,0.632781680116511),
 .UNSPECIFIED.)
CURVE()
GEOMETRIC_REPRESENTATION_ITEM()
RATIONAL_B_SPLINE_CURVE((1.03767852232438,1.17702201605488,1.03767852232437))
REPRESENTATION_ITEM('')
);
#1358=(
BOUNDED_CURVE()
B_SPLINE_CURVE(2,(#33796,#33797,#33798),.UNSPECIFIED.,.F.,.F.)
B_SPLINE_CURVE_WITH_KNOTS((3,3),(0.0681231928610322,0.632781680116511),
 .UNSPECIFIED.)
CURVE()
GEOMETRIC_REPRESENTATION_ITEM()
RATIONAL_B_SPLINE_CURVE((1.03767852232438,1.17702201605488,1.03767852232437))
REPRESENTATION_ITEM('')
);
#1359=(
BOUNDED_CURVE()
B_SPLINE_CURVE(2,(#33800,#33801,#33802),.UNSPECIFIED.,.F.,.F.)
B_SPLINE_CURVE_WITH_KNOTS((3,3),(0.0681231928610319,0.632781680116511),
 .UNSPECIFIED.)
CURVE()
GEOMETRIC_REPRESENTATION_ITEM()
RATIONAL_B_SPLINE_CURVE((1.03767852232438,1.17702201605488,1.03767852232438))
REPRESENTATION_ITEM('')
);
#1360=(
BOUNDED_CURVE()
B_SPLINE_CURVE(2,(#33806,#33807,#33808),.UNSPECIFIED.,.F.,.F.)
B_SPLINE_CURVE_WITH_KNOTS((3,3),(0.0681231928610319,0.350452436488771),
 .UNSPECIFIED.)
CURVE()
GEOMETRIC_REPRESENTATION_ITEM()
RATIONAL_B_SPLINE_CURVE((1.03767852232438,1.10735026918963,1.10735026918963))
REPRESENTATION_ITEM('')
);
#1361=(
BOUNDED_CURVE()
B_SPLINE_CURVE(2,(#33809,#33810,#33811),.UNSPECIFIED.,.F.,.F.)
B_SPLINE_CURVE_WITH_KNOTS((3,3),(0.068123192861032,0.632781680116511),
 .UNSPECIFIED.)
CURVE()
GEOMETRIC_REPRESENTATION_ITEM()
RATIONAL_B_SPLINE_CURVE((1.03767852232437,1.17702201605488,1.03767852232437))
REPRESENTATION_ITEM('')
);
#1362=(
BOUNDED_CURVE()
B_SPLINE_CURVE(2,(#33812,#33813,#33814),.UNSPECIFIED.,.F.,.F.)
B_SPLINE_CURVE_WITH_KNOTS((3,3),(0.0681231928610317,0.632781680116511),
 .UNSPECIFIED.)
CURVE()
GEOMETRIC_REPRESENTATION_ITEM()
RATIONAL_B_SPLINE_CURVE((1.03767852232438,1.17702201605488,1.03767852232438))
REPRESENTATION_ITEM('')
);
#1363=(
BOUNDED_CURVE()
B_SPLINE_CURVE(2,(#33815,#33816,#33817),.UNSPECIFIED.,.F.,.F.)
B_SPLINE_CURVE_WITH_KNOTS((3,3),(0.350452436488771,0.632781680116511),
 .UNSPECIFIED.)
CURVE()
GEOMETRIC_REPRESENTATION_ITEM()
RATIONAL_B_SPLINE_CURVE((1.10735026918963,1.10735026918963,1.03767852232438))
REPRESENTATION_ITEM('')
);
#1364=(
BOUNDED_CURVE()
B_SPLINE_CURVE(2,(#37805,#37806,#37807),.UNSPECIFIED.,.F.,.F.)
B_SPLINE_CURVE_WITH_KNOTS((3,3),(0.,0.0331882448287731),.UNSPECIFIED.)
CURVE()
GEOMETRIC_REPRESENTATION_ITEM()
RATIONAL_B_SPLINE_CURVE((1.,1.00036538368932,1.))
REPRESENTATION_ITEM('')
);
#1365=(
BOUNDED_CURVE()
B_SPLINE_CURVE(2,(#37819,#37820,#37821),.UNSPECIFIED.,.F.,.F.)
B_SPLINE_CURVE_WITH_KNOTS((3,3),(0.,0.0331882448287731),.UNSPECIFIED.)
CURVE()
GEOMETRIC_REPRESENTATION_ITEM()
RATIONAL_B_SPLINE_CURVE((1.,1.00036538368669,1.))
REPRESENTATION_ITEM('')
);
#1366=(
BOUNDED_CURVE()
B_SPLINE_CURVE(2,(#38064,#38065,#38066),.UNSPECIFIED.,.F.,.F.)
B_SPLINE_CURVE_WITH_KNOTS((3,3),(0.,0.033188244828773),.UNSPECIFIED.)
CURVE()
GEOMETRIC_REPRESENTATION_ITEM()
RATIONAL_B_SPLINE_CURVE((1.,1.00036538369005,1.))
REPRESENTATION_ITEM('')
);
#1367=(
BOUNDED_CURVE()
B_SPLINE_CURVE(2,(#38073,#38074,#38075),.UNSPECIFIED.,.F.,.F.)
B_SPLINE_CURVE_WITH_KNOTS((3,3),(0.,0.0331882448287731),.UNSPECIFIED.)
CURVE()
GEOMETRIC_REPRESENTATION_ITEM()
RATIONAL_B_SPLINE_CURVE((1.,1.00036538368877,1.))
REPRESENTATION_ITEM('')
);
#1368=(
BOUNDED_CURVE()
B_SPLINE_CURVE(2,(#38078,#38079,#38080),.UNSPECIFIED.,.F.,.F.)
B_SPLINE_CURVE_WITH_KNOTS((3,3),(0.,0.0331882448287731),.UNSPECIFIED.)
CURVE()
GEOMETRIC_REPRESENTATION_ITEM()
RATIONAL_B_SPLINE_CURVE((1.,1.00036538368768,1.))
REPRESENTATION_ITEM('')
);
#1369=(
BOUNDED_CURVE()
B_SPLINE_CURVE(2,(#38087,#38088,#38089),.UNSPECIFIED.,.F.,.F.)
B_SPLINE_CURVE_WITH_KNOTS((3,3),(0.,0.0331882448287732),.UNSPECIFIED.)
CURVE()
GEOMETRIC_REPRESENTATION_ITEM()
RATIONAL_B_SPLINE_CURVE((1.,1.00036538368663,1.))
REPRESENTATION_ITEM('')
);
#1370=(
BOUNDED_CURVE()
B_SPLINE_CURVE(2,(#38092,#38093,#38094),.UNSPECIFIED.,.F.,.F.)
B_SPLINE_CURVE_WITH_KNOTS((3,3),(0.,0.033188244828773),.UNSPECIFIED.)
CURVE()
GEOMETRIC_REPRESENTATION_ITEM()
RATIONAL_B_SPLINE_CURVE((1.,1.0003653836895,1.))
REPRESENTATION_ITEM('')
);
#1371=(
BOUNDED_CURVE()
B_SPLINE_CURVE(2,(#38101,#38102,#38103),.UNSPECIFIED.,.F.,.F.)
B_SPLINE_CURVE_WITH_KNOTS((3,3),(0.,0.0331882448287732),.UNSPECIFIED.)
CURVE()
GEOMETRIC_REPRESENTATION_ITEM()
RATIONAL_B_SPLINE_CURVE((1.,1.0003653836875,1.))
REPRESENTATION_ITEM('')
);
#1372=(
BOUNDED_CURVE()
B_SPLINE_CURVE(2,(#38106,#38107,#38108),.UNSPECIFIED.,.F.,.F.)
B_SPLINE_CURVE_WITH_KNOTS((3,3),(0.,0.0331882448287729),.UNSPECIFIED.)
CURVE()
GEOMETRIC_REPRESENTATION_ITEM()
RATIONAL_B_SPLINE_CURVE((1.,1.00036538368829,1.))
REPRESENTATION_ITEM('')
);
#1373=(
BOUNDED_CURVE()
B_SPLINE_CURVE(2,(#38115,#38116,#38117),.UNSPECIFIED.,.F.,.F.)
B_SPLINE_CURVE_WITH_KNOTS((3,3),(0.,0.0331882448287728),.UNSPECIFIED.)
CURVE()
GEOMETRIC_REPRESENTATION_ITEM()
RATIONAL_B_SPLINE_CURVE((1.,1.00036538369157,1.))
REPRESENTATION_ITEM('')
);
#1374=(
BOUNDED_CURVE()
B_SPLINE_CURVE(2,(#38120,#38121,#38122),.UNSPECIFIED.,.F.,.F.)
B_SPLINE_CURVE_WITH_KNOTS((3,3),(0.,0.0331882448287729),.UNSPECIFIED.)
CURVE()
GEOMETRIC_REPRESENTATION_ITEM()
RATIONAL_B_SPLINE_CURVE((1.,1.00036538368829,1.))
REPRESENTATION_ITEM('')
);
#1375=(
BOUNDED_CURVE()
B_SPLINE_CURVE(2,(#38129,#38130,#38131),.UNSPECIFIED.,.F.,.F.)
B_SPLINE_CURVE_WITH_KNOTS((3,3),(0.,0.0331882448287729),.UNSPECIFIED.)
CURVE()
GEOMETRIC_REPRESENTATION_ITEM()
RATIONAL_B_SPLINE_CURVE((1.,1.00036538368924,1.))
REPRESENTATION_ITEM('')
);
#1376=(
BOUNDED_CURVE()
B_SPLINE_CURVE(2,(#38134,#38135,#38136),.UNSPECIFIED.,.F.,.F.)
B_SPLINE_CURVE_WITH_KNOTS((3,3),(0.,0.033188244828773),.UNSPECIFIED.)
CURVE()
GEOMETRIC_REPRESENTATION_ITEM()
RATIONAL_B_SPLINE_CURVE((1.,1.0003653836883,1.))
REPRESENTATION_ITEM('')
);
#1377=(
BOUNDED_CURVE()
B_SPLINE_CURVE(2,(#38143,#38144,#38145),.UNSPECIFIED.,.F.,.F.)
B_SPLINE_CURVE_WITH_KNOTS((3,3),(0.,0.033188244828773),.UNSPECIFIED.)
CURVE()
GEOMETRIC_REPRESENTATION_ITEM()
RATIONAL_B_SPLINE_CURVE((1.,1.00036538368856,1.))
REPRESENTATION_ITEM('')
);
#1378=(
BOUNDED_CURVE()
B_SPLINE_CURVE(2,(#38148,#38149,#38150),.UNSPECIFIED.,.F.,.F.)
B_SPLINE_CURVE_WITH_KNOTS((3,3),(0.,0.0331882448287729),.UNSPECIFIED.)
CURVE()
GEOMETRIC_REPRESENTATION_ITEM()
RATIONAL_B_SPLINE_CURVE((1.,1.000365383688,1.))
REPRESENTATION_ITEM('')
);
#1379=(
BOUNDED_CURVE()
B_SPLINE_CURVE(2,(#38157,#38158,#38159),.UNSPECIFIED.,.F.,.F.)
B_SPLINE_CURVE_WITH_KNOTS((3,3),(0.,0.0331882448287729),.UNSPECIFIED.)
CURVE()
GEOMETRIC_REPRESENTATION_ITEM()
RATIONAL_B_SPLINE_CURVE((1.,1.00036538369129,1.))
REPRESENTATION_ITEM('')
);
#1380=(
BOUNDED_CURVE()
B_SPLINE_CURVE(2,(#38162,#38163,#38164),.UNSPECIFIED.,.F.,.F.)
B_SPLINE_CURVE_WITH_KNOTS((3,3),(0.,0.033188244828773),.UNSPECIFIED.)
CURVE()
GEOMETRIC_REPRESENTATION_ITEM()
RATIONAL_B_SPLINE_CURVE((1.,1.00036538369007,1.))
REPRESENTATION_ITEM('')
);
#1381=(
BOUNDED_CURVE()
B_SPLINE_CURVE(2,(#38171,#38172,#38173),.UNSPECIFIED.,.F.,.F.)
B_SPLINE_CURVE_WITH_KNOTS((3,3),(0.,0.0331882448287728),.UNSPECIFIED.)
CURVE()
GEOMETRIC_REPRESENTATION_ITEM()
RATIONAL_B_SPLINE_CURVE((1.,1.00036538369054,1.))
REPRESENTATION_ITEM('')
);
#1382=(
BOUNDED_CURVE()
B_SPLINE_CURVE(2,(#38176,#38177,#38178),.UNSPECIFIED.,.F.,.F.)
B_SPLINE_CURVE_WITH_KNOTS((3,3),(0.,0.0331882448287728),.UNSPECIFIED.)
CURVE()
GEOMETRIC_REPRESENTATION_ITEM()
RATIONAL_B_SPLINE_CURVE((1.,1.00036538369027,1.))
REPRESENTATION_ITEM('')
);
#1383=(
BOUNDED_CURVE()
B_SPLINE_CURVE(2,(#38185,#38186,#38187),.UNSPECIFIED.,.F.,.F.)
B_SPLINE_CURVE_WITH_KNOTS((3,3),(0.,0.033188244828773),.UNSPECIFIED.)
CURVE()
GEOMETRIC_REPRESENTATION_ITEM()
RATIONAL_B_SPLINE_CURVE((1.,1.00036538369294,1.))
REPRESENTATION_ITEM('')
);
#1384=(
BOUNDED_CURVE()
B_SPLINE_CURVE(2,(#38190,#38191,#38192),.UNSPECIFIED.,.F.,.F.)
B_SPLINE_CURVE_WITH_KNOTS((3,3),(0.,0.0331882448287729),.UNSPECIFIED.)
CURVE()
GEOMETRIC_REPRESENTATION_ITEM()
RATIONAL_B_SPLINE_CURVE((1.,1.00036538369069,1.))
REPRESENTATION_ITEM('')
);
#1385=(
BOUNDED_CURVE()
B_SPLINE_CURVE(2,(#38199,#38200,#38201),.UNSPECIFIED.,.F.,.F.)
B_SPLINE_CURVE_WITH_KNOTS((3,3),(0.,0.0331882448287729),.UNSPECIFIED.)
CURVE()
GEOMETRIC_REPRESENTATION_ITEM()
RATIONAL_B_SPLINE_CURVE((1.,1.00036538369006,1.))
REPRESENTATION_ITEM('')
);
#1386=(
BOUNDED_CURVE()
B_SPLINE_CURVE(2,(#38204,#38205,#38206),.UNSPECIFIED.,.F.,.F.)
B_SPLINE_CURVE_WITH_KNOTS((3,3),(0.,0.0331882448287728),.UNSPECIFIED.)
CURVE()
GEOMETRIC_REPRESENTATION_ITEM()
RATIONAL_B_SPLINE_CURVE((1.,1.00036538369315,1.))
REPRESENTATION_ITEM('')
);
#1387=(
BOUNDED_CURVE()
B_SPLINE_CURVE(2,(#38213,#38214,#38215),.UNSPECIFIED.,.F.,.F.)
B_SPLINE_CURVE_WITH_KNOTS((3,3),(0.,0.0331882448287729),.UNSPECIFIED.)
CURVE()
GEOMETRIC_REPRESENTATION_ITEM()
RATIONAL_B_SPLINE_CURVE((1.,1.00036538368966,1.))
REPRESENTATION_ITEM('')
);
#1388=(
BOUNDED_CURVE()
B_SPLINE_CURVE(2,(#38218,#38219,#38220),.UNSPECIFIED.,.F.,.F.)
B_SPLINE_CURVE_WITH_KNOTS((3,3),(0.,0.0331882448287729),.UNSPECIFIED.)
CURVE()
GEOMETRIC_REPRESENTATION_ITEM()
RATIONAL_B_SPLINE_CURVE((1.,1.00036538369197,1.))
REPRESENTATION_ITEM('')
);
#1389=(
BOUNDED_CURVE()
B_SPLINE_CURVE(2,(#38227,#38228,#38229),.UNSPECIFIED.,.F.,.F.)
B_SPLINE_CURVE_WITH_KNOTS((3,3),(0.,0.0331882448287729),.UNSPECIFIED.)
CURVE()
GEOMETRIC_REPRESENTATION_ITEM()
RATIONAL_B_SPLINE_CURVE((1.,1.00036538368905,1.))
REPRESENTATION_ITEM('')
);
#1390=(
BOUNDED_CURVE()
B_SPLINE_CURVE(2,(#38232,#38233,#38234),.UNSPECIFIED.,.F.,.F.)
B_SPLINE_CURVE_WITH_KNOTS((3,3),(0.,0.033188244828773),.UNSPECIFIED.)
CURVE()
GEOMETRIC_REPRESENTATION_ITEM()
RATIONAL_B_SPLINE_CURVE((1.,1.0003653836867,1.))
REPRESENTATION_ITEM('')
);
#1391=(
BOUNDED_CURVE()
B_SPLINE_CURVE(2,(#38241,#38242,#38243),.UNSPECIFIED.,.F.,.F.)
B_SPLINE_CURVE_WITH_KNOTS((3,3),(0.,0.0331882448287729),.UNSPECIFIED.)
CURVE()
GEOMETRIC_REPRESENTATION_ITEM()
RATIONAL_B_SPLINE_CURVE((1.,1.00036538369137,1.))
REPRESENTATION_ITEM('')
);
#1392=(
BOUNDED_CURVE()
B_SPLINE_CURVE(2,(#38246,#38247,#38248),.UNSPECIFIED.,.F.,.F.)
B_SPLINE_CURVE_WITH_KNOTS((3,3),(0.,0.033188244828773),.UNSPECIFIED.)
CURVE()
GEOMETRIC_REPRESENTATION_ITEM()
RATIONAL_B_SPLINE_CURVE((1.,1.0003653836899,1.))
REPRESENTATION_ITEM('')
);
#1393=(
BOUNDED_CURVE()
B_SPLINE_CURVE(2,(#38255,#38256,#38257),.UNSPECIFIED.,.F.,.F.)
B_SPLINE_CURVE_WITH_KNOTS((3,3),(0.,0.033188244828773),.UNSPECIFIED.)
CURVE()
GEOMETRIC_REPRESENTATION_ITEM()
RATIONAL_B_SPLINE_CURVE((1.,1.00036538369,1.))
REPRESENTATION_ITEM('')
);
#1394=(
BOUNDED_CURVE()
B_SPLINE_CURVE(2,(#38260,#38261,#38262),.UNSPECIFIED.,.F.,.F.)
B_SPLINE_CURVE_WITH_KNOTS((3,3),(0.,0.0331882448287729),.UNSPECIFIED.)
CURVE()
GEOMETRIC_REPRESENTATION_ITEM()
RATIONAL_B_SPLINE_CURVE((1.,1.00036538369195,1.))
REPRESENTATION_ITEM('')
);
#1395=(
BOUNDED_CURVE()
B_SPLINE_CURVE(2,(#38269,#38270,#38271),.UNSPECIFIED.,.F.,.F.)
B_SPLINE_CURVE_WITH_KNOTS((3,3),(0.,0.033188244828773),.UNSPECIFIED.)
CURVE()
GEOMETRIC_REPRESENTATION_ITEM()
RATIONAL_B_SPLINE_CURVE((1.,1.00036538369028,1.))
REPRESENTATION_ITEM('')
);
#1396=(
BOUNDED_CURVE()
B_SPLINE_CURVE(2,(#38274,#38275,#38276),.UNSPECIFIED.,.F.,.F.)
B_SPLINE_CURVE_WITH_KNOTS((3,3),(0.,0.0331882448287728),.UNSPECIFIED.)
CURVE()
GEOMETRIC_REPRESENTATION_ITEM()
RATIONAL_B_SPLINE_CURVE((1.,1.00036538369196,1.))
REPRESENTATION_ITEM('')
);
#1397=(
BOUNDED_CURVE()
B_SPLINE_CURVE(2,(#38283,#38284,#38285),.UNSPECIFIED.,.F.,.F.)
B_SPLINE_CURVE_WITH_KNOTS((3,3),(0.,0.0331882448287729),.UNSPECIFIED.)
CURVE()
GEOMETRIC_REPRESENTATION_ITEM()
RATIONAL_B_SPLINE_CURVE((1.,1.00036538369028,1.))
REPRESENTATION_ITEM('')
);
#1398=(
BOUNDED_CURVE()
B_SPLINE_CURVE(2,(#38288,#38289,#38290),.UNSPECIFIED.,.F.,.F.)
B_SPLINE_CURVE_WITH_KNOTS((3,3),(0.,0.0331882448287729),.UNSPECIFIED.)
CURVE()
GEOMETRIC_REPRESENTATION_ITEM()
RATIONAL_B_SPLINE_CURVE((1.,1.00036538369004,1.))
REPRESENTATION_ITEM('')
);
#1399=(
BOUNDED_CURVE()
B_SPLINE_CURVE(2,(#38297,#38298,#38299),.UNSPECIFIED.,.F.,.F.)
B_SPLINE_CURVE_WITH_KNOTS((3,3),(0.,0.033188244828773),.UNSPECIFIED.)
CURVE()
GEOMETRIC_REPRESENTATION_ITEM()
RATIONAL_B_SPLINE_CURVE((1.,1.00036538368968,1.))
REPRESENTATION_ITEM('')
);
#1400=(
BOUNDED_CURVE()
B_SPLINE_CURVE(2,(#38302,#38303,#38304),.UNSPECIFIED.,.F.,.F.)
B_SPLINE_CURVE_WITH_KNOTS((3,3),(0.,0.0331882448287729),.UNSPECIFIED.)
CURVE()
GEOMETRIC_REPRESENTATION_ITEM()
RATIONAL_B_SPLINE_CURVE((1.,1.0003653836908,1.))
REPRESENTATION_ITEM('')
);
#1401=(
BOUNDED_CURVE()
B_SPLINE_CURVE(2,(#38311,#38312,#38313),.UNSPECIFIED.,.F.,.F.)
B_SPLINE_CURVE_WITH_KNOTS((3,3),(0.,0.0331882448287729),.UNSPECIFIED.)
CURVE()
GEOMETRIC_REPRESENTATION_ITEM()
RATIONAL_B_SPLINE_CURVE((1.,1.00036538369234,1.))
REPRESENTATION_ITEM('')
);
#1402=(
BOUNDED_CURVE()
B_SPLINE_CURVE(2,(#38316,#38317,#38318),.UNSPECIFIED.,.F.,.F.)
B_SPLINE_CURVE_WITH_KNOTS((3,3),(0.,0.033188244828773),.UNSPECIFIED.)
CURVE()
GEOMETRIC_REPRESENTATION_ITEM()
RATIONAL_B_SPLINE_CURVE((1.,1.00036538368982,1.))
REPRESENTATION_ITEM('')
);
#1403=(
BOUNDED_CURVE()
B_SPLINE_CURVE(2,(#38325,#38326,#38327),.UNSPECIFIED.,.F.,.F.)
B_SPLINE_CURVE_WITH_KNOTS((3,3),(0.,0.0331882448287727),.UNSPECIFIED.)
CURVE()
GEOMETRIC_REPRESENTATION_ITEM()
RATIONAL_B_SPLINE_CURVE((1.,1.00036538368872,1.))
REPRESENTATION_ITEM('')
);
#1404=(
BOUNDED_CURVE()
B_SPLINE_CURVE(2,(#38330,#38331,#38332),.UNSPECIFIED.,.F.,.F.)
B_SPLINE_CURVE_WITH_KNOTS((3,3),(0.,0.0331882448287729),.UNSPECIFIED.)
CURVE()
GEOMETRIC_REPRESENTATION_ITEM()
RATIONAL_B_SPLINE_CURVE((1.,1.00036538368741,1.))
REPRESENTATION_ITEM('')
);
#1405=(
BOUNDED_CURVE()
B_SPLINE_CURVE(2,(#38339,#38340,#38341),.UNSPECIFIED.,.F.,.F.)
B_SPLINE_CURVE_WITH_KNOTS((3,3),(0.,0.0331882448287729),.UNSPECIFIED.)
CURVE()
GEOMETRIC_REPRESENTATION_ITEM()
RATIONAL_B_SPLINE_CURVE((1.,1.00036538369134,1.))
REPRESENTATION_ITEM('')
);
#1406=(
BOUNDED_CURVE()
B_SPLINE_CURVE(2,(#38344,#38345,#38346),.UNSPECIFIED.,.F.,.F.)
B_SPLINE_CURVE_WITH_KNOTS((3,3),(0.,0.0331882448287729),.UNSPECIFIED.)
CURVE()
GEOMETRIC_REPRESENTATION_ITEM()
RATIONAL_B_SPLINE_CURVE((1.,1.00036538368855,1.))
REPRESENTATION_ITEM('')
);
#1407=(
BOUNDED_CURVE()
B_SPLINE_CURVE(2,(#38353,#38354,#38355),.UNSPECIFIED.,.F.,.F.)
B_SPLINE_CURVE_WITH_KNOTS((3,3),(0.,0.0331882448287729),.UNSPECIFIED.)
CURVE()
GEOMETRIC_REPRESENTATION_ITEM()
RATIONAL_B_SPLINE_CURVE((1.,1.00036538368991,1.))
REPRESENTATION_ITEM('')
);
#1408=(
BOUNDED_CURVE()
B_SPLINE_CURVE(2,(#38358,#38359,#38360),.UNSPECIFIED.,.F.,.F.)
B_SPLINE_CURVE_WITH_KNOTS((3,3),(0.,0.0331882448287729),.UNSPECIFIED.)
CURVE()
GEOMETRIC_REPRESENTATION_ITEM()
RATIONAL_B_SPLINE_CURVE((1.,1.00036538369097,1.))
REPRESENTATION_ITEM('')
);
#1409=(
BOUNDED_CURVE()
B_SPLINE_CURVE(2,(#38367,#38368,#38369),.UNSPECIFIED.,.F.,.F.)
B_SPLINE_CURVE_WITH_KNOTS((3,3),(0.,0.0331882448287729),.UNSPECIFIED.)
CURVE()
GEOMETRIC_REPRESENTATION_ITEM()
RATIONAL_B_SPLINE_CURVE((1.,1.00036538369135,1.))
REPRESENTATION_ITEM('')
);
#1410=(
BOUNDED_CURVE()
B_SPLINE_CURVE(2,(#38372,#38373,#38374),.UNSPECIFIED.,.F.,.F.)
B_SPLINE_CURVE_WITH_KNOTS((3,3),(0.,0.033188244828773),.UNSPECIFIED.)
CURVE()
GEOMETRIC_REPRESENTATION_ITEM()
RATIONAL_B_SPLINE_CURVE((1.,1.00036538369049,1.))
REPRESENTATION_ITEM('')
);
#1411=(
BOUNDED_CURVE()
B_SPLINE_CURVE(2,(#38381,#38382,#38383),.UNSPECIFIED.,.F.,.F.)
B_SPLINE_CURVE_WITH_KNOTS((3,3),(0.,0.033188244828773),.UNSPECIFIED.)
CURVE()
GEOMETRIC_REPRESENTATION_ITEM()
RATIONAL_B_SPLINE_CURVE((1.,1.00036538369154,1.))
REPRESENTATION_ITEM('')
);
#1412=(
BOUNDED_CURVE()
B_SPLINE_CURVE(2,(#38386,#38387,#38388),.UNSPECIFIED.,.F.,.F.)
B_SPLINE_CURVE_WITH_KNOTS((3,3),(0.,0.0331882448287728),.UNSPECIFIED.)
CURVE()
GEOMETRIC_REPRESENTATION_ITEM()
RATIONAL_B_SPLINE_CURVE((1.,1.00036538368967,1.))
REPRESENTATION_ITEM('')
);
#1413=(
BOUNDED_CURVE()
B_SPLINE_CURVE(2,(#38395,#38396,#38397),.UNSPECIFIED.,.F.,.F.)
B_SPLINE_CURVE_WITH_KNOTS((3,3),(0.,0.033188244828773),.UNSPECIFIED.)
CURVE()
GEOMETRIC_REPRESENTATION_ITEM()
RATIONAL_B_SPLINE_CURVE((1.,1.00036538369075,1.))
REPRESENTATION_ITEM('')
);
#1414=(
BOUNDED_CURVE()
B_SPLINE_CURVE(2,(#38400,#38401,#38402),.UNSPECIFIED.,.F.,.F.)
B_SPLINE_CURVE_WITH_KNOTS((3,3),(0.,0.0331882448287729),.UNSPECIFIED.)
CURVE()
GEOMETRIC_REPRESENTATION_ITEM()
RATIONAL_B_SPLINE_CURVE((1.,1.00036538369014,1.))
REPRESENTATION_ITEM('')
);
#1415=(
BOUNDED_CURVE()
B_SPLINE_CURVE(2,(#38409,#38410,#38411),.UNSPECIFIED.,.F.,.F.)
B_SPLINE_CURVE_WITH_KNOTS((3,3),(0.,0.0331882448287729),.UNSPECIFIED.)
CURVE()
GEOMETRIC_REPRESENTATION_ITEM()
RATIONAL_B_SPLINE_CURVE((1.,1.00036538368956,1.))
REPRESENTATION_ITEM('')
);
#1416=(
BOUNDED_CURVE()
B_SPLINE_CURVE(2,(#38414,#38415,#38416),.UNSPECIFIED.,.F.,.F.)
B_SPLINE_CURVE_WITH_KNOTS((3,3),(0.,0.0331882448287729),.UNSPECIFIED.)
CURVE()
GEOMETRIC_REPRESENTATION_ITEM()
RATIONAL_B_SPLINE_CURVE((1.,1.00036538369215,1.))
REPRESENTATION_ITEM('')
);
#1417=(
BOUNDED_CURVE()
B_SPLINE_CURVE(2,(#38423,#38424,#38425),.UNSPECIFIED.,.F.,.F.)
B_SPLINE_CURVE_WITH_KNOTS((3,3),(0.,0.0331882448287728),.UNSPECIFIED.)
CURVE()
GEOMETRIC_REPRESENTATION_ITEM()
RATIONAL_B_SPLINE_CURVE((1.,1.00036538368934,1.))
REPRESENTATION_ITEM('')
);
#1418=(
BOUNDED_CURVE()
B_SPLINE_CURVE(2,(#38428,#38429,#38430),.UNSPECIFIED.,.F.,.F.)
B_SPLINE_CURVE_WITH_KNOTS((3,3),(0.,0.0331882448287729),.UNSPECIFIED.)
CURVE()
GEOMETRIC_REPRESENTATION_ITEM()
RATIONAL_B_SPLINE_CURVE((1.,1.00036538368812,1.))
REPRESENTATION_ITEM('')
);
#1419=(
BOUNDED_CURVE()
B_SPLINE_CURVE(2,(#38437,#38438,#38439),.UNSPECIFIED.,.F.,.F.)
B_SPLINE_CURVE_WITH_KNOTS((3,3),(0.,0.033188244828773),.UNSPECIFIED.)
CURVE()
GEOMETRIC_REPRESENTATION_ITEM()
RATIONAL_B_SPLINE_CURVE((1.,1.00036538368966,1.))
REPRESENTATION_ITEM('')
);
#1420=(
BOUNDED_CURVE()
B_SPLINE_CURVE(2,(#38442,#38443,#38444),.UNSPECIFIED.,.F.,.F.)
B_SPLINE_CURVE_WITH_KNOTS((3,3),(0.,0.033188244828773),.UNSPECIFIED.)
CURVE()
GEOMETRIC_REPRESENTATION_ITEM()
RATIONAL_B_SPLINE_CURVE((1.,1.00036538368713,1.))
REPRESENTATION_ITEM('')
);
#1421=(
BOUNDED_CURVE()
B_SPLINE_CURVE(2,(#38451,#38452,#38453),.UNSPECIFIED.,.F.,.F.)
B_SPLINE_CURVE_WITH_KNOTS((3,3),(0.,0.0331882448287729),.UNSPECIFIED.)
CURVE()
GEOMETRIC_REPRESENTATION_ITEM()
RATIONAL_B_SPLINE_CURVE((1.,1.00036538369046,1.))
REPRESENTATION_ITEM('')
);
#1422=(
BOUNDED_CURVE()
B_SPLINE_CURVE(2,(#38456,#38457,#38458),.UNSPECIFIED.,.F.,.F.)
B_SPLINE_CURVE_WITH_KNOTS((3,3),(0.,0.033188244828773),.UNSPECIFIED.)
CURVE()
GEOMETRIC_REPRESENTATION_ITEM()
RATIONAL_B_SPLINE_CURVE((1.,1.00036538369035,1.))
REPRESENTATION_ITEM('')
);
#1423=(
BOUNDED_CURVE()
B_SPLINE_CURVE(2,(#38465,#38466,#38467),.UNSPECIFIED.,.F.,.F.)
B_SPLINE_CURVE_WITH_KNOTS((3,3),(0.,0.033188244828773),.UNSPECIFIED.)
CURVE()
GEOMETRIC_REPRESENTATION_ITEM()
RATIONAL_B_SPLINE_CURVE((1.,1.00036538369101,1.))
REPRESENTATION_ITEM('')
);
#1424=ELLIPSE('',#17244,96.0000000000002,48.);
#1425=ELLIPSE('',#17247,96.0000000000002,48.);
#1426=ELLIPSE('',#17252,96.,48.);
#1427=ELLIPSE('',#17254,66.5459160514177,47.0550685002283);
#1428=ELLIPSE('',#17259,8.48528137423855,6.);
#1429=ELLIPSE('',#17261,8.48528137423855,6.);
#1430=ELLIPSE('',#17268,66.5459160514174,47.0550685002282);
#1431=ELLIPSE('',#17285,96.,48.);
#1432=FACE_BOUND('',#3270,.T.);
#1433=FACE_BOUND('',#3271,.T.);
#1434=FACE_BOUND('',#3272,.T.);
#1435=FACE_BOUND('',#3273,.T.);
#1436=FACE_BOUND('',#3300,.T.);
#1437=FACE_BOUND('',#3301,.T.);
#1438=FACE_BOUND('',#3321,.T.);
#1439=FACE_BOUND('',#3329,.T.);
#1440=FACE_BOUND('',#3330,.T.);
#1441=FACE_BOUND('',#3331,.T.);
#1442=FACE_BOUND('',#3336,.T.);
#1443=FACE_BOUND('',#3408,.T.);
#1444=FACE_BOUND('',#3855,.T.);
#1445=FACE_BOUND('',#3859,.T.);
#1446=FACE_BOUND('',#3860,.T.);
#1447=FACE_BOUND('',#3861,.T.);
#1448=FACE_BOUND('',#3862,.T.);
#1449=FACE_BOUND('',#3863,.T.);
#1450=FACE_BOUND('',#3864,.T.);
#1451=FACE_BOUND('',#3989,.T.);
#1452=FACE_BOUND('',#3990,.T.);
#1453=FACE_BOUND('',#3991,.T.);
#1454=FACE_BOUND('',#3992,.T.);
#1455=FACE_BOUND('',#3993,.T.);
#1456=FACE_BOUND('',#3994,.T.);
#1457=FACE_BOUND('',#3995,.T.);
#1458=FACE_BOUND('',#3996,.T.);
#1459=FACE_BOUND('',#3997,.T.);
#1460=FACE_BOUND('',#3998,.T.);
#1461=FACE_BOUND('',#3999,.T.);
#1462=FACE_BOUND('',#4028,.T.);
#1463=FACE_BOUND('',#4032,.T.);
#1464=FACE_BOUND('',#4036,.T.);
#1465=FACE_BOUND('',#4058,.T.);
#1466=FACE_BOUND('',#4065,.T.);
#1467=FACE_BOUND('',#4071,.T.);
#1468=FACE_BOUND('',#4074,.T.);
#1469=FACE_BOUND('',#4078,.T.);
#1470=FACE_BOUND('',#4081,.T.);
#1471=FACE_BOUND('',#4085,.T.);
#1472=FACE_BOUND('',#4088,.T.);
#1473=FACE_BOUND('',#4093,.T.);
#1474=FACE_BOUND('',#4096,.T.);
#1475=FACE_BOUND('',#4158,.T.);
#1476=FACE_BOUND('',#4287,.T.);
#1477=CIRCLE('',#17226,48.);
#1478=CIRCLE('',#17227,48.);
#1479=CIRCLE('',#17256,48.);
#1480=CIRCLE('',#17257,47.5);
#1481=CIRCLE('',#17260,6.);
#1482=CIRCLE('',#17263,47.5);
#1483=CIRCLE('',#17264,3.05);
#1484=CIRCLE('',#17265,11.5);
#1485=CIRCLE('',#17267,48.);
#1486=CIRCLE('',#17280,2.55);
#1487=CIRCLE('',#17282,2.55);
#1488=CIRCLE('',#17290,2.55);
#1489=CIRCLE('',#17292,47.6464466094067);
#1490=CIRCLE('',#17293,48.);
#1491=CIRCLE('',#17295,47.5535533905933);
#1492=CIRCLE('',#17298,11.);
#1493=CIRCLE('',#17300,11.);
#1494=CIRCLE('',#17302,46.7);
#1495=CIRCLE('',#17304,11.6);
#1496=CIRCLE('',#17305,5.);
#1497=CIRCLE('',#17306,2.05);
#1498=CIRCLE('',#17309,2.55);
#1499=CIRCLE('',#17312,2.05);
#1500=CIRCLE('',#17315,5.);
#1501=CIRCLE('',#17326,53.5);
#1502=CIRCLE('',#17327,53.5);
#1503=CIRCLE('',#17329,53.);
#1504=CIRCLE('',#17332,53.5);
#1505=CIRCLE('',#17333,53.5);
#1506=CIRCLE('',#17335,53.);
#1507=CIRCLE('',#17338,0.700000000000003);
#1508=CIRCLE('',#17339,0.700000000000003);
#1509=CIRCLE('',#17342,0.700000000000003);
#1510=CIRCLE('',#17343,1.2);
#1511=CIRCLE('',#17345,0.700000000000003);
#1512=CIRCLE('',#17348,0.700000000000003);
#1513=CIRCLE('',#17349,0.700000000000003);
#1514=CIRCLE('',#17351,1.2);
#1515=CIRCLE('',#17354,0.700000000000003);
#1516=CIRCLE('',#17355,1.2);
#1517=CIRCLE('',#17357,0.700000000000003);
#1518=CIRCLE('',#17362,0.700000000000003);
#1519=CIRCLE('',#17363,0.700000000000003);
#1520=CIRCLE('',#17365,53.5);
#1521=CIRCLE('',#17366,53.);
#1522=CIRCLE('',#17369,53.5);
#1523=CIRCLE('',#17370,53.5);
#1524=CIRCLE('',#17372,53.);
#1525=CIRCLE('',#17375,53.5);
#1526=CIRCLE('',#17376,53.);
#1527=CIRCLE('',#17378,53.5);
#1528=CIRCLE('',#17382,53.5);
#1529=CIRCLE('',#17383,53.);
#1530=CIRCLE('',#17385,53.5);
#1531=CIRCLE('',#17389,53.5);
#1532=CIRCLE('',#17390,53.);
#1533=CIRCLE('',#17392,53.5);
#1534=CIRCLE('',#17396,53.5);
#1535=CIRCLE('',#17397,53.);
#1536=CIRCLE('',#17399,53.5);
#1537=CIRCLE('',#17403,53.5);
#1538=CIRCLE('',#17404,53.);
#1539=CIRCLE('',#17406,53.5);
#1540=CIRCLE('',#17410,53.5);
#1541=CIRCLE('',#17411,53.);
#1542=CIRCLE('',#17413,53.5);
#1543=CIRCLE('',#17417,53.5);
#1544=CIRCLE('',#17418,53.);
#1545=CIRCLE('',#17420,53.5);
#1546=CIRCLE('',#17424,53.5);
#1547=CIRCLE('',#17425,53.);
#1548=CIRCLE('',#17427,53.5);
#1549=CIRCLE('',#17430,0.700000000000003);
#1550=CIRCLE('',#17431,1.2);
#1551=CIRCLE('',#17433,53.);
#1552=CIRCLE('',#17434,53.5);
#1553=CIRCLE('',#17436,53.);
#1554=CIRCLE('',#17437,53.5);
#1555=CIRCLE('',#17439,53.5);
#1556=CIRCLE('',#17440,53.);
#1557=CIRCLE('',#17442,0.700000000000003);
#1558=CIRCLE('',#17443,53.);
#1559=CIRCLE('',#17444,0.700000000000003);
#1560=CIRCLE('',#17445,53.);
#1561=CIRCLE('',#17446,0.700000000000003);
#1562=CIRCLE('',#17447,53.);
#1563=CIRCLE('',#17448,0.700000000000003);
#1564=CIRCLE('',#17449,53.);
#1565=CIRCLE('',#17450,0.700000000000003);
#1566=CIRCLE('',#17451,53.);
#1567=CIRCLE('',#17452,0.700000000000003);
#1568=CIRCLE('',#17453,53.);
#1569=CIRCLE('',#17454,0.700000000000003);
#1570=CIRCLE('',#17455,1.2);
#1571=CIRCLE('',#17456,1.2);
#1572=CIRCLE('',#17457,1.2);
#1573=CIRCLE('',#17458,1.2);
#1574=CIRCLE('',#17459,1.2);
#1575=CIRCLE('',#17460,1.2);
#1576=CIRCLE('',#17461,1.2);
#1577=CIRCLE('',#17462,1.2);
#1578=CIRCLE('',#17463,53.);
#1579=CIRCLE('',#17464,1.2);
#1580=CIRCLE('',#17465,53.);
#1581=CIRCLE('',#17466,1.2);
#1582=CIRCLE('',#17467,53.);
#1583=CIRCLE('',#17468,1.2);
#1584=CIRCLE('',#17469,53.);
#1585=CIRCLE('',#17470,1.2);
#1586=CIRCLE('',#17471,53.);
#1587=CIRCLE('',#17472,1.20000000000001);
#1588=CIRCLE('',#17473,53.);
#1589=CIRCLE('',#17474,1.2);
#1590=CIRCLE('',#17475,53.);
#1591=CIRCLE('',#17476,1.2);
#1592=CIRCLE('',#17477,53.);
#1593=CIRCLE('',#17478,1.2);
#1594=CIRCLE('',#17479,53.);
#1595=CIRCLE('',#17480,1.2);
#1596=CIRCLE('',#17481,0.700000000000003);
#1597=CIRCLE('',#17482,53.);
#1598=CIRCLE('',#17483,0.700000000000003);
#1599=CIRCLE('',#17484,53.);
#1600=CIRCLE('',#17485,1.2);
#1601=CIRCLE('',#17486,53.);
#1602=CIRCLE('',#17487,1.2);
#1603=CIRCLE('',#17488,53.);
#1604=CIRCLE('',#17489,1.2);
#1605=CIRCLE('',#17490,53.);
#1606=CIRCLE('',#17491,1.2);
#1607=CIRCLE('',#17492,53.);
#1608=CIRCLE('',#17493,1.20000000000001);
#1609=CIRCLE('',#17494,53.);
#1610=CIRCLE('',#17495,1.2);
#1611=CIRCLE('',#17496,53.);
#1612=CIRCLE('',#17497,1.2);
#1613=CIRCLE('',#17498,53.);
#1614=CIRCLE('',#17499,1.2);
#1615=CIRCLE('',#17500,53.);
#1616=CIRCLE('',#17501,0.700000000000003);
#1617=CIRCLE('',#17502,53.);
#1618=CIRCLE('',#17503,1.2);
#1619=CIRCLE('',#17504,53.);
#1620=CIRCLE('',#17505,0.700000000000003);
#1621=CIRCLE('',#17506,53.);
#1622=CIRCLE('',#17507,1.2);
#1623=CIRCLE('',#17508,53.);
#1624=CIRCLE('',#17509,1.2);
#1625=CIRCLE('',#17510,53.);
#1626=CIRCLE('',#17511,1.2);
#1627=CIRCLE('',#17512,53.);
#1628=CIRCLE('',#17513,1.2);
#1629=CIRCLE('',#17514,53.);
#1630=CIRCLE('',#17515,1.2);
#1631=CIRCLE('',#17516,53.);
#1632=CIRCLE('',#17517,1.2);
#1633=CIRCLE('',#17518,53.);
#1634=CIRCLE('',#17519,1.2);
#1635=CIRCLE('',#17520,53.);
#1636=CIRCLE('',#17521,0.700000000000003);
#1637=CIRCLE('',#17522,53.);
#1638=CIRCLE('',#17523,1.2);
#1639=CIRCLE('',#17524,53.);
#1640=CIRCLE('',#17525,1.2);
#1641=CIRCLE('',#17526,53.);
#1642=CIRCLE('',#17527,0.700000000000003);
#1643=CIRCLE('',#17528,53.);
#1644=CIRCLE('',#17529,1.2);
#1645=CIRCLE('',#17530,53.);
#1646=CIRCLE('',#17531,1.2);
#1647=CIRCLE('',#17532,53.);
#1648=CIRCLE('',#17533,1.2);
#1649=CIRCLE('',#17534,53.);
#1650=CIRCLE('',#17535,1.2);
#1651=CIRCLE('',#17536,53.);
#1652=CIRCLE('',#17537,1.2);
#1653=CIRCLE('',#17538,53.);
#1654=CIRCLE('',#17539,1.2);
#1655=CIRCLE('',#17540,53.);
#1656=CIRCLE('',#17541,0.700000000000003);
#1657=CIRCLE('',#17542,53.);
#1658=CIRCLE('',#17543,1.2);
#1659=CIRCLE('',#17544,53.);
#1660=CIRCLE('',#17545,1.20000000000001);
#1661=CIRCLE('',#17546,53.);
#1662=CIRCLE('',#17547,1.2);
#1663=CIRCLE('',#17548,53.);
#1664=CIRCLE('',#17549,0.700000000000003);
#1665=CIRCLE('',#17550,53.);
#1666=CIRCLE('',#17551,1.2);
#1667=CIRCLE('',#17552,53.);
#1668=CIRCLE('',#17553,1.2);
#1669=CIRCLE('',#17554,53.);
#1670=CIRCLE('',#17555,1.2);
#1671=CIRCLE('',#17556,53.);
#1672=CIRCLE('',#17557,1.2);
#1673=CIRCLE('',#17558,53.);
#1674=CIRCLE('',#17559,1.2);
#1675=CIRCLE('',#17560,53.);
#1676=CIRCLE('',#17561,0.700000000000003);
#1677=CIRCLE('',#17562,53.);
#1678=CIRCLE('',#17563,1.2);
#1679=CIRCLE('',#17564,53.);
#1680=CIRCLE('',#17565,1.2);
#1681=CIRCLE('',#17566,53.);
#1682=CIRCLE('',#17567,1.2);
#1683=CIRCLE('',#17568,53.);
#1684=CIRCLE('',#17569,1.2);
#1685=CIRCLE('',#17570,53.);
#1686=CIRCLE('',#17571,0.700000000000003);
#1687=CIRCLE('',#17572,53.);
#1688=CIRCLE('',#17573,1.20000000000001);
#1689=CIRCLE('',#17574,53.);
#1690=CIRCLE('',#17575,1.2);
#1691=CIRCLE('',#17576,53.);
#1692=CIRCLE('',#17577,1.2);
#1693=CIRCLE('',#17578,53.);
#1694=CIRCLE('',#17579,1.2);
#1695=CIRCLE('',#17580,53.);
#1696=CIRCLE('',#17581,0.700000000000003);
#1697=CIRCLE('',#17582,53.);
#1698=CIRCLE('',#17583,1.20000000000001);
#1699=CIRCLE('',#17584,53.);
#1700=CIRCLE('',#17585,1.2);
#1701=CIRCLE('',#17586,53.);
#1702=CIRCLE('',#17587,1.2);
#1703=CIRCLE('',#17588,53.);
#1704=CIRCLE('',#17589,1.2);
#1705=CIRCLE('',#17590,53.);
#1706=CIRCLE('',#17591,1.2);
#1707=CIRCLE('',#17592,53.);
#1708=CIRCLE('',#17593,0.700000000000003);
#1709=CIRCLE('',#17594,53.);
#1710=CIRCLE('',#17595,1.2);
#1711=CIRCLE('',#17596,53.);
#1712=CIRCLE('',#17597,1.2);
#1713=CIRCLE('',#17598,53.);
#1714=CIRCLE('',#17599,1.20000000000001);
#1715=CIRCLE('',#17600,53.);
#1716=CIRCLE('',#17601,50.);
#1717=CIRCLE('',#17603,0.700000000000003);
#1718=CIRCLE('',#17607,0.700000000000003);
#1719=CIRCLE('',#17609,0.700000000000003);
#1720=CIRCLE('',#17613,0.700000000000003);
#1721=CIRCLE('',#17615,0.700000000000003);
#1722=CIRCLE('',#17619,0.700000000000003);
#1723=CIRCLE('',#17621,0.700000000000003);
#1724=CIRCLE('',#17624,53.5);
#1725=CIRCLE('',#17625,53.5);
#1726=CIRCLE('',#17630,53.5);
#1727=CIRCLE('',#17632,53.5);
#1728=CIRCLE('',#17636,53.5);
#1729=CIRCLE('',#17638,53.5);
#1730=CIRCLE('',#17642,53.5);
#1731=CIRCLE('',#17644,53.5);
#1732=CIRCLE('',#17648,53.5);
#1733=CIRCLE('',#17650,53.5);
#1734=CIRCLE('',#17654,53.5);
#1735=CIRCLE('',#17656,53.5);
#1736=CIRCLE('',#17660,53.5);
#1737=CIRCLE('',#17662,53.5);
#1738=CIRCLE('',#17665,53.5);
#1739=CIRCLE('',#17667,53.5);
#1740=CIRCLE('',#17669,53.5);
#1741=CIRCLE('',#17671,53.5);
#1742=CIRCLE('',#17673,53.5);
#1743=CIRCLE('',#17675,53.5);
#1744=CIRCLE('',#17678,0.700000000000003);
#1745=CIRCLE('',#17680,0.700000000000003);
#1746=CIRCLE('',#17682,0.700000000000003);
#1747=CIRCLE('',#17684,0.700000000000003);
#1748=CIRCLE('',#17686,0.700000000000003);
#1749=CIRCLE('',#17688,0.700000000000003);
#1750=CIRCLE('',#17690,0.700000000000003);
#1751=CIRCLE('',#17692,0.700000000000003);
#1752=CIRCLE('',#17694,0.700000000000003);
#1753=CIRCLE('',#17696,0.700000000000003);
#1754=CIRCLE('',#17698,0.700000000000003);
#1755=CIRCLE('',#17701,0.700000000000003);
#1756=CIRCLE('',#17703,0.700000000000003);
#1757=CIRCLE('',#17706,53.5);
#1758=CIRCLE('',#17709,0.700000000000003);
#1759=CIRCLE('',#17711,0.700000000000003);
#1760=CIRCLE('',#17715,0.700000000000003);
#1761=CIRCLE('',#17717,0.700000000000003);
#1762=CIRCLE('',#17721,0.700000000000003);
#1763=CIRCLE('',#17723,0.700000000000003);
#1764=CIRCLE('',#17726,53.5);
#1765=CIRCLE('',#17727,53.5);
#1766=CIRCLE('',#17732,53.5);
#1767=CIRCLE('',#17734,53.5);
#1768=CIRCLE('',#17738,53.5);
#1769=CIRCLE('',#17740,53.5);
#1770=CIRCLE('',#17744,53.5);
#1771=CIRCLE('',#17746,53.5);
#1772=CIRCLE('',#17750,53.5);
#1773=CIRCLE('',#17752,53.5);
#1774=CIRCLE('',#17756,53.5);
#1775=CIRCLE('',#17758,53.5);
#1776=CIRCLE('',#17761,53.5);
#1777=CIRCLE('',#17763,53.5);
#1778=CIRCLE('',#17765,53.5);
#1779=CIRCLE('',#17767,53.5);
#1780=CIRCLE('',#17769,53.5);
#1781=CIRCLE('',#17771,53.5);
#1782=CIRCLE('',#17773,53.5);
#1783=CIRCLE('',#17776,0.700000000000003);
#1784=CIRCLE('',#17778,0.700000000000003);
#1785=CIRCLE('',#17780,0.700000000000003);
#1786=CIRCLE('',#17782,0.700000000000003);
#1787=CIRCLE('',#17784,0.700000000000003);
#1788=CIRCLE('',#17786,0.700000000000003);
#1789=CIRCLE('',#17788,0.700000000000003);
#1790=CIRCLE('',#17790,0.700000000000003);
#1791=CIRCLE('',#17792,0.700000000000003);
#1792=CIRCLE('',#17795,0.700000000000003);
#1793=CIRCLE('',#17797,0.700000000000003);
#1794=CIRCLE('',#17801,0.700000000000003);
#1795=CIRCLE('',#17803,0.700000000000003);
#1796=CIRCLE('',#17807,0.700000000000003);
#1797=CIRCLE('',#17809,0.700000000000003);
#1798=CIRCLE('',#17813,0.700000000000003);
#1799=CIRCLE('',#17815,0.700000000000003);
#1800=CIRCLE('',#17819,0.700000000000003);
#1801=CIRCLE('',#17821,0.700000000000003);
#1802=CIRCLE('',#17824,53.5);
#1803=CIRCLE('',#17825,53.5);
#1804=CIRCLE('',#17830,53.5);
#1805=CIRCLE('',#17832,53.5);
#1806=CIRCLE('',#17836,53.5);
#1807=CIRCLE('',#17838,53.5);
#1808=CIRCLE('',#17842,53.5);
#1809=CIRCLE('',#17844,53.5);
#1810=CIRCLE('',#17848,53.5);
#1811=CIRCLE('',#17850,53.5);
#1812=CIRCLE('',#17853,53.5);
#1813=CIRCLE('',#17855,53.5);
#1814=CIRCLE('',#17857,53.5);
#1815=CIRCLE('',#17859,53.5);
#1816=CIRCLE('',#17861,53.5);
#1817=CIRCLE('',#17863,53.5);
#1818=CIRCLE('',#17865,53.5);
#1819=CIRCLE('',#17867,53.5);
#1820=CIRCLE('',#17869,53.5);
#1821=CIRCLE('',#17871,53.5);
#1822=CIRCLE('',#17874,0.700000000000003);
#1823=CIRCLE('',#17876,0.700000000000003);
#1824=CIRCLE('',#17878,0.700000000000003);
#1825=CIRCLE('',#17880,0.700000000000003);
#1826=CIRCLE('',#17882,0.700000000000003);
#1827=CIRCLE('',#17884,0.700000000000003);
#1828=CIRCLE('',#17886,0.700000000000003);
#1829=CIRCLE('',#17889,0.700000000000003);
#1830=CIRCLE('',#17891,0.700000000000003);
#1831=CIRCLE('',#17894,53.5);
#1832=CIRCLE('',#17897,0.700000000000003);
#1833=CIRCLE('',#17899,0.700000000000003);
#1834=CIRCLE('',#17903,0.700000000000003);
#1835=CIRCLE('',#17905,0.700000000000003);
#1836=CIRCLE('',#17909,0.700000000000003);
#1837=CIRCLE('',#17911,0.700000000000003);
#1838=CIRCLE('',#17915,0.700000000000003);
#1839=CIRCLE('',#17917,0.700000000000003);
#1840=CIRCLE('',#17921,0.700000000000003);
#1841=CIRCLE('',#17923,0.700000000000003);
#1842=CIRCLE('',#17926,53.5);
#1843=CIRCLE('',#17927,53.5);
#1844=CIRCLE('',#17932,53.5);
#1845=CIRCLE('',#17934,53.5);
#1846=CIRCLE('',#17938,53.5);
#1847=CIRCLE('',#17940,53.5);
#1848=CIRCLE('',#17944,53.5);
#1849=CIRCLE('',#17946,53.5);
#1850=CIRCLE('',#17949,53.5);
#1851=CIRCLE('',#17951,53.5);
#1852=CIRCLE('',#17953,53.5);
#1853=CIRCLE('',#17955,53.5);
#1854=CIRCLE('',#17957,53.5);
#1855=CIRCLE('',#17959,53.5);
#1856=CIRCLE('',#17961,53.5);
#1857=CIRCLE('',#17963,53.5);
#1858=CIRCLE('',#17965,53.5);
#1859=CIRCLE('',#17967,53.5);
#1860=CIRCLE('',#17969,53.5);
#1861=CIRCLE('',#17972,0.700000000000003);
#1862=CIRCLE('',#17974,0.700000000000003);
#1863=CIRCLE('',#17976,0.700000000000003);
#1864=CIRCLE('',#17978,0.700000000000003);
#1865=CIRCLE('',#17980,0.700000000000003);
#1866=CIRCLE('',#17983,0.700000000000003);
#1867=CIRCLE('',#17985,0.700000000000003);
#1868=CIRCLE('',#17989,0.700000000000003);
#1869=CIRCLE('',#17991,0.700000000000003);
#1870=CIRCLE('',#17995,0.700000000000003);
#1871=CIRCLE('',#17997,0.700000000000003);
#1872=CIRCLE('',#18001,0.700000000000003);
#1873=CIRCLE('',#18003,0.700000000000003);
#1874=CIRCLE('',#18007,0.700000000000003);
#1875=CIRCLE('',#18009,0.700000000000003);
#1876=CIRCLE('',#18013,0.700000000000003);
#1877=CIRCLE('',#18015,0.700000000000003);
#1878=CIRCLE('',#18019,0.700000000000003);
#1879=CIRCLE('',#18021,0.700000000000003);
#1880=CIRCLE('',#18024,53.5);
#1881=CIRCLE('',#18025,53.5);
#1882=CIRCLE('',#18030,53.5);
#1883=CIRCLE('',#18032,53.5);
#1884=CIRCLE('',#18036,53.5);
#1885=CIRCLE('',#18038,53.5);
#1886=CIRCLE('',#18041,53.5);
#1887=CIRCLE('',#18043,53.5);
#1888=CIRCLE('',#18045,53.5);
#1889=CIRCLE('',#18047,53.5);
#1890=CIRCLE('',#18049,53.5);
#1891=CIRCLE('',#18051,53.5);
#1892=CIRCLE('',#18053,53.5);
#1893=CIRCLE('',#18055,53.5);
#1894=CIRCLE('',#18057,53.5);
#1895=CIRCLE('',#18059,53.5);
#1896=CIRCLE('',#18061,53.5);
#1897=CIRCLE('',#18063,53.5);
#1898=CIRCLE('',#18065,53.5);
#1899=CIRCLE('',#18067,53.5);
#1900=CIRCLE('',#18070,0.700000000000003);
#1901=CIRCLE('',#18072,0.700000000000003);
#1902=CIRCLE('',#18074,0.700000000000003);
#1903=CIRCLE('',#18077,0.700000000000003);
#1904=CIRCLE('',#18079,0.700000000000003);
#1905=CIRCLE('',#18083,0.700000000000003);
#1906=CIRCLE('',#18085,0.700000000000003);
#1907=CIRCLE('',#18089,0.700000000000003);
#1908=CIRCLE('',#18091,0.700000000000003);
#1909=CIRCLE('',#18095,0.700000000000003);
#1910=CIRCLE('',#18097,0.700000000000003);
#1911=CIRCLE('',#18101,0.700000000000003);
#1912=CIRCLE('',#18103,0.700000000000003);
#1913=CIRCLE('',#18107,0.700000000000003);
#1914=CIRCLE('',#18109,0.700000000000003);
#1915=CIRCLE('',#18113,0.700000000000003);
#1916=CIRCLE('',#18115,0.700000000000003);
#1917=CIRCLE('',#18119,0.700000000000003);
#1918=CIRCLE('',#18121,0.700000000000003);
#1919=CIRCLE('',#18124,53.5);
#1920=CIRCLE('',#18125,53.5);
#1921=CIRCLE('',#18130,53.5);
#1922=CIRCLE('',#18132,53.5);
#1923=CIRCLE('',#18135,53.5);
#1924=CIRCLE('',#18137,53.5);
#1925=CIRCLE('',#18139,53.5);
#1926=CIRCLE('',#18141,53.5);
#1927=CIRCLE('',#18143,53.5);
#1928=CIRCLE('',#18145,53.5);
#1929=CIRCLE('',#18147,53.5);
#1930=CIRCLE('',#18149,53.5);
#1931=CIRCLE('',#18151,53.5);
#1932=CIRCLE('',#18153,53.5);
#1933=CIRCLE('',#18155,53.5);
#1934=CIRCLE('',#18157,53.5);
#1935=CIRCLE('',#18159,53.5);
#1936=CIRCLE('',#18161,53.5);
#1937=CIRCLE('',#18163,53.5);
#1938=CIRCLE('',#18165,53.5);
#1939=CIRCLE('',#18168,0.700000000000003);
#1940=CIRCLE('',#18171,53.5);
#1941=CIRCLE('',#18173,53.5);
#1942=CIRCLE('',#18177,53.5);
#1943=CIRCLE('',#18179,53.5);
#1944=CIRCLE('',#18183,53.5);
#1945=CIRCLE('',#18185,53.5);
#1946=CIRCLE('',#18189,53.5);
#1947=CIRCLE('',#18191,53.5);
#1948=CIRCLE('',#18195,53.5);
#1949=CIRCLE('',#18197,53.5);
#1950=CIRCLE('',#18201,53.5);
#1951=CIRCLE('',#18203,53.5);
#1952=CIRCLE('',#18207,53.5);
#1953=CIRCLE('',#18209,53.5);
#1954=CIRCLE('',#18213,53.5);
#1955=CIRCLE('',#18215,53.5);
#1956=CIRCLE('',#18219,53.5);
#1957=CIRCLE('',#18221,53.5);
#1958=CIRCLE('',#18224,0.700000000000003);
#1959=CIRCLE('',#18225,0.700000000000003);
#1960=CIRCLE('',#18229,0.700000000000003);
#1961=CIRCLE('',#18231,0.700000000000003);
#1962=CIRCLE('',#18233,0.700000000000003);
#1963=CIRCLE('',#18235,0.700000000000003);
#1964=CIRCLE('',#18237,0.700000000000003);
#1965=CIRCLE('',#18239,0.700000000000003);
#1966=CIRCLE('',#18241,0.700000000000003);
#1967=CIRCLE('',#18243,0.700000000000003);
#1968=CIRCLE('',#18245,0.700000000000003);
#1969=CIRCLE('',#18247,0.700000000000003);
#1970=CIRCLE('',#18249,0.700000000000003);
#1971=CIRCLE('',#18251,0.700000000000003);
#1972=CIRCLE('',#18253,0.700000000000003);
#1973=CIRCLE('',#18255,0.700000000000003);
#1974=CIRCLE('',#18257,0.700000000000003);
#1975=CIRCLE('',#18259,0.700000000000003);
#1976=CIRCLE('',#18261,49.5);
#1977=CIRCLE('',#18263,49.5);
#1978=CIRCLE('',#18266,0.700000000000003);
#1979=CIRCLE('',#18268,0.700000000000003);
#1980=CIRCLE('',#18270,0.700000000000003);
#1981=CIRCLE('',#18272,0.700000000000003);
#1982=CIRCLE('',#18274,0.700000000000003);
#1983=CIRCLE('',#18276,0.700000000000003);
#1984=CIRCLE('',#18278,0.700000000000003);
#1985=CIRCLE('',#18280,0.700000000000003);
#1986=CIRCLE('',#18282,0.700000000000003);
#1987=CIRCLE('',#18284,0.700000000000003);
#1988=CIRCLE('',#18286,0.700000000000003);
#1989=CIRCLE('',#18288,0.700000000000003);
#1990=CIRCLE('',#18290,0.700000000000003);
#1991=CIRCLE('',#18292,0.700000000000003);
#1992=CIRCLE('',#18294,0.700000000000003);
#1993=CIRCLE('',#18296,0.700000000000003);
#1994=CIRCLE('',#18298,0.700000000000003);
#1995=CIRCLE('',#18301,0.700000000000003);
#1996=CIRCLE('',#18304,53.5);
#1997=CIRCLE('',#18307,0.700000000000003);
#1998=CIRCLE('',#18310,53.5);
#1999=CIRCLE('',#18313,0.700000000000003);
#2000=CIRCLE('',#18316,53.5);
#2001=CIRCLE('',#18319,0.700000000000003);
#2002=CIRCLE('',#18322,53.5);
#2003=CIRCLE('',#18325,0.700000000000003);
#2004=CIRCLE('',#18328,53.5);
#2005=CIRCLE('',#18331,0.700000000000003);
#2006=CIRCLE('',#18334,53.5);
#2007=CIRCLE('',#18337,53.0535533905933);
#2008=CIRCLE('',#18338,52.2);
#2009=CIRCLE('',#18340,51.1);
#2010=CIRCLE('',#18342,53.5);
#2011=CIRCLE('',#18343,53.5);
#2012=CIRCLE('',#18344,53.5);
#2013=CIRCLE('',#18345,53.5);
#2014=CIRCLE('',#18346,53.5);
#2015=CIRCLE('',#18347,53.5);
#2016=CIRCLE('',#18348,53.5);
#2017=CIRCLE('',#18349,53.5);
#2018=CIRCLE('',#18350,53.5);
#2019=CIRCLE('',#18351,53.5);
#2020=CIRCLE('',#18352,53.5);
#2021=CIRCLE('',#18353,53.5);
#2022=CIRCLE('',#18354,53.5);
#2023=CIRCLE('',#18355,53.5);
#2024=CIRCLE('',#18356,53.5);
#2025=CIRCLE('',#18357,53.5);
#2026=CIRCLE('',#18358,53.5);
#2027=CIRCLE('',#18359,53.5);
#2028=CIRCLE('',#18360,53.5);
#2029=CIRCLE('',#18361,53.5);
#2030=CIRCLE('',#18362,53.5);
#2031=CIRCLE('',#18363,53.5);
#2032=CIRCLE('',#18364,53.5);
#2033=CIRCLE('',#18365,53.5);
#2034=CIRCLE('',#18366,53.5);
#2035=CIRCLE('',#18367,53.5);
#2036=CIRCLE('',#18368,53.5);
#2037=CIRCLE('',#18369,53.5);
#2038=CIRCLE('',#18370,53.5);
#2039=CIRCLE('',#18371,53.5);
#2040=CIRCLE('',#18372,53.5);
#2041=CIRCLE('',#18373,53.5);
#2042=CIRCLE('',#18374,53.5);
#2043=CIRCLE('',#18375,53.5);
#2044=CIRCLE('',#18376,53.5);
#2045=CIRCLE('',#18377,53.5);
#2046=CIRCLE('',#18378,53.5);
#2047=CIRCLE('',#18379,53.5);
#2048=CIRCLE('',#18380,53.5);
#2049=CIRCLE('',#18381,53.5);
#2050=CIRCLE('',#18382,53.5);
#2051=CIRCLE('',#18383,53.5);
#2052=CIRCLE('',#18384,53.5);
#2053=CIRCLE('',#18385,53.5);
#2054=CIRCLE('',#18386,53.5);
#2055=CIRCLE('',#18387,53.5);
#2056=CIRCLE('',#18388,53.5);
#2057=CIRCLE('',#18389,53.5);
#2058=CIRCLE('',#18390,53.5);
#2059=CIRCLE('',#18391,53.5);
#2060=CIRCLE('',#18392,53.5);
#2061=CIRCLE('',#18393,53.5);
#2062=CIRCLE('',#18394,53.5);
#2063=CIRCLE('',#18395,53.5);
#2064=CIRCLE('',#18396,53.5);
#2065=CIRCLE('',#18397,53.5);
#2066=CIRCLE('',#18398,53.5);
#2067=CIRCLE('',#18399,53.5);
#2068=CIRCLE('',#18400,53.5);
#2069=CIRCLE('',#18401,53.5);
#2070=CIRCLE('',#18402,53.5);
#2071=CIRCLE('',#18403,53.5);
#2072=CIRCLE('',#18404,53.5);
#2073=CIRCLE('',#18405,53.5);
#2074=CIRCLE('',#18406,53.5);
#2075=CIRCLE('',#18407,53.5);
#2076=CIRCLE('',#18408,53.5);
#2077=CIRCLE('',#18409,53.5);
#2078=CIRCLE('',#18410,53.5);
#2079=CIRCLE('',#18411,53.5);
#2080=CIRCLE('',#18412,53.5);
#2081=CIRCLE('',#18413,53.5);
#2082=CIRCLE('',#18414,53.5);
#2083=CIRCLE('',#18415,53.5);
#2084=CIRCLE('',#18416,53.5);
#2085=CIRCLE('',#18417,53.5);
#2086=CIRCLE('',#18418,53.5);
#2087=CIRCLE('',#18419,53.5);
#2088=CIRCLE('',#18420,53.5);
#2089=CIRCLE('',#18421,53.5);
#2090=CIRCLE('',#18422,53.5);
#2091=CIRCLE('',#18423,53.5);
#2092=CIRCLE('',#18424,53.5);
#2093=CIRCLE('',#18425,53.5);
#2094=CIRCLE('',#18426,53.5);
#2095=CIRCLE('',#18427,53.5);
#2096=CIRCLE('',#18428,53.5);
#2097=CIRCLE('',#18429,53.5);
#2098=CIRCLE('',#18430,53.5);
#2099=CIRCLE('',#18431,53.5);
#2100=CIRCLE('',#18432,53.5);
#2101=CIRCLE('',#18433,53.5);
#2102=CIRCLE('',#18434,53.5);
#2103=CIRCLE('',#18435,53.5);
#2104=CIRCLE('',#18436,53.5);
#2105=CIRCLE('',#18437,53.5);
#2106=CIRCLE('',#18438,53.5);
#2107=CIRCLE('',#18439,53.5);
#2108=CIRCLE('',#18440,53.5);
#2109=CIRCLE('',#18441,53.5);
#2110=CIRCLE('',#18442,53.5);
#2111=CIRCLE('',#18444,12.9);
#2112=CIRCLE('',#18445,12.5);
#2113=CIRCLE('',#18447,50.5);
#2114=CIRCLE('',#18448,12.9);
#2115=CIRCLE('',#18449,12.9);
#2116=CIRCLE('',#18450,5.025);
#2117=CIRCLE('',#18451,12.9);
#2118=CIRCLE('',#18452,12.9);
#2119=CIRCLE('',#18454,12.5);
#2120=CIRCLE('',#18456,12.5);
#2121=CIRCLE('',#18458,12.5);
#2122=CIRCLE('',#18460,12.5);
#2123=CIRCLE('',#18462,12.5);
#2124=CIRCLE('',#18464,12.5);
#2125=CIRCLE('',#18466,12.5);
#2126=CIRCLE('',#18468,12.5);
#2127=CIRCLE('',#18470,12.5);
#2128=CIRCLE('',#18472,50.5);
#2129=CIRCLE('',#18491,0.700000000000003);
#2130=CIRCLE('',#18503,0.700000000000003);
#2131=CIRCLE('',#18515,0.700000000000003);
#2132=CIRCLE('',#18557,0.700000000000003);
#2133=CIRCLE('',#18569,0.700000000000003);
#2134=CIRCLE('',#18581,0.700000000000003);
#2135=CIRCLE('',#18587,1.5);
#2136=CIRCLE('',#18589,1.5);
#2137=CIRCLE('',#18591,1.5);
#2138=CIRCLE('',#18593,1.5);
#2139=CIRCLE('',#18595,1.5);
#2140=CIRCLE('',#18597,5.025);
#2141=CIRCLE('',#18601,9.64155);
#2142=CIRCLE('',#18613,9.64155);
#2143=CIRCLE('',#18615,10.06205);
#2144=CIRCLE('',#18627,10.06205);
#2145=CIRCLE('',#18630,12.5);
#2146=CIRCLE('',#18633,12.5);
#2147=CIRCLE('',#18635,13.5);
#2148=CIRCLE('',#18637,13.5);
#2149=CIRCLE('',#18639,13.1);
#2150=CIRCLE('',#18643,2.942);
#2151=CIRCLE('',#18650,2.37175);
#2152=CIRCLE('',#18657,2.942);
#2153=CIRCLE('',#18658,2.942);
#2154=CIRCLE('',#18660,2.37175);
#2155=CIRCLE('',#18662,2.942);
#2156=CIRCLE('',#18664,4.6);
#2157=CIRCLE('',#18666,5.);
#2158=CIRCLE('',#18668,5.);
#2159=CIRCLE('',#18671,2.6);
#2160=CIRCLE('',#18675,9.2422018555175);
#2161=CIRCLE('',#18676,9.2422018555175);
#2162=CIRCLE('',#18677,9.89294404963443);
#2163=CIRCLE('',#18678,9.89294404963443);
#2164=CIRCLE('',#18680,11.);
#2165=CIRCLE('',#18682,6.);
#2166=CIRCLE('',#18684,5.6);
#2167=CIRCLE('',#18685,5.);
#2168=CIRCLE('',#18687,5.6);
#2169=CIRCLE('',#18689,5.);
#2170=CIRCLE('',#18692,8.2);
#2171=CIRCLE('',#18693,8.2);
#2172=CIRCLE('',#18695,11.);
#2173=CIRCLE('',#18701,5.25);
#2174=CIRCLE('',#18702,5.25);
#2175=CIRCLE('',#18704,12.);
#2176=CIRCLE('',#18706,12.);
#2177=CIRCLE('',#18710,5.8);
#2178=CIRCLE('',#18711,6.);
#2179=CIRCLE('',#18712,6.);
#2180=CIRCLE('',#18714,6.);
#2181=CIRCLE('',#18716,3.2);
#2182=CIRCLE('',#18718,3.2);
#2183=CIRCLE('',#18720,5.8);
#2184=CIRCLE('',#18724,3.26);
#2185=CIRCLE('',#18725,3.05);
#2186=CIRCLE('',#18727,3.05);
#2187=CIRCLE('',#18729,4.76709676493043);
#2188=CIRCLE('',#18731,3.26);
#2189=CIRCLE('',#18733,4.55709676493043);
#2190=CIRCLE('',#18735,4.94836613655247);
#2191=CIRCLE('',#18736,4.94836613655247);
#2192=CIRCLE('',#18737,4.94836613655247);
#2193=CIRCLE('',#18738,4.94836613655247);
#2194=CIRCLE('',#18739,4.94836613655247);
#2195=CIRCLE('',#18740,4.94836613655247);
#2196=CIRCLE('',#18768,2.);
#2197=CIRCLE('',#18770,0.25);
#2198=CIRCLE('',#18771,0.25);
#2199=CIRCLE('',#18776,2.4505);
#2200=CIRCLE('',#18781,1.99475);
#2201=CIRCLE('',#18786,2.4505);
#2202=CIRCLE('',#18787,2.4505);
#2203=CIRCLE('',#18789,2.4505);
#2204=CIRCLE('',#18790,2.4505);
#2205=CIRCLE('',#18791,1.99475);
#2206=CIRCLE('',#18801,2.);
#2207=CIRCLE('',#18804,2.4505);
#2208=CIRCLE('',#18806,2.2);
#2209=CIRCLE('',#18810,2.4505);
#2210=CIRCLE('',#18826,1.99475);
#2211=CIRCLE('',#18841,2.4505);
#2212=CIRCLE('',#18842,2.4505);
#2213=CIRCLE('',#18843,1.99475);
#2214=CIRCLE('',#18847,5.);
#2215=CIRCLE('',#18850,5.);
#2216=CIRCLE('',#18851,5.);
#2217=CIRCLE('',#18852,5.);
#2218=CIRCLE('',#18853,5.);
#2219=CIRCLE('',#18854,5.);
#2220=CIRCLE('',#18855,5.);
#2221=CIRCLE('',#18856,5.);
#2222=CIRCLE('',#18857,5.);
#2223=CIRCLE('',#18858,5.);
#2224=CIRCLE('',#18859,5.);
#2225=CIRCLE('',#18860,5.);
#2226=CIRCLE('',#18861,5.);
#2227=CIRCLE('',#18862,5.);
#2228=CIRCLE('',#18863,5.);
#2229=CIRCLE('',#18864,5.);
#2230=CIRCLE('',#18865,5.);
#2231=CIRCLE('',#18866,5.);
#2232=CIRCLE('',#18867,5.);
#2233=CIRCLE('',#18868,5.);
#2234=CIRCLE('',#18869,5.);
#2235=CIRCLE('',#18870,5.);
#2236=CIRCLE('',#18871,5.);
#2237=CIRCLE('',#18872,5.);
#2238=CIRCLE('',#18873,5.);
#2239=CIRCLE('',#18874,5.);
#2240=CIRCLE('',#18875,5.);
#2241=CIRCLE('',#18876,5.);
#2242=CIRCLE('',#18877,5.);
#2243=CIRCLE('',#18878,5.);
#2244=CIRCLE('',#18879,5.);
#2245=CIRCLE('',#18880,5.);
#2246=CIRCLE('',#18881,5.);
#2247=CIRCLE('',#18882,5.);
#2248=CIRCLE('',#18883,5.);
#2249=CIRCLE('',#18884,5.);
#2250=CIRCLE('',#18885,5.);
#2251=CIRCLE('',#18886,5.);
#2252=CIRCLE('',#18887,5.);
#2253=CIRCLE('',#18888,5.);
#2254=CIRCLE('',#18889,5.);
#2255=CIRCLE('',#18890,5.);
#2256=CIRCLE('',#18891,5.);
#2257=CIRCLE('',#18892,5.);
#2258=CIRCLE('',#18893,5.);
#2259=CIRCLE('',#18894,5.);
#2260=CIRCLE('',#18895,5.);
#2261=CIRCLE('',#18896,5.);
#2262=CIRCLE('',#18897,5.);
#2263=CIRCLE('',#18898,5.);
#2264=CIRCLE('',#18899,5.);
#2265=CIRCLE('',#18900,5.);
#2266=CIRCLE('',#18901,5.);
#2267=CIRCLE('',#18902,5.);
#2268=CIRCLE('',#18903,5.);
#2269=CIRCLE('',#18904,5.);
#2270=CIRCLE('',#18905,5.);
#2271=CIRCLE('',#18906,5.);
#2272=CIRCLE('',#18907,5.);
#2273=CIRCLE('',#18908,5.);
#2274=CIRCLE('',#18909,5.);
#2275=CIRCLE('',#18910,5.);
#2276=CIRCLE('',#18999,2.1);
#2277=CIRCLE('',#19002,2.4505);
#2278=CIRCLE('',#19004,4.5);
#2279=CIRCLE('',#19007,4.4);
#2280=FACE_OUTER_BOUND('',#3263,.T.);
#2281=FACE_OUTER_BOUND('',#3264,.T.);
#2282=FACE_OUTER_BOUND('',#3265,.T.);
#2283=FACE_OUTER_BOUND('',#3266,.T.);
#2284=FACE_OUTER_BOUND('',#3267,.T.);
#2285=FACE_OUTER_BOUND('',#3268,.T.);
#2286=FACE_OUTER_BOUND('',#3269,.T.);
#2287=FACE_OUTER_BOUND('',#3274,.T.);
#2288=FACE_OUTER_BOUND('',#3275,.T.);
#2289=FACE_OUTER_BOUND('',#3276,.T.);
#2290=FACE_OUTER_BOUND('',#3277,.T.);
#2291=FACE_OUTER_BOUND('',#3278,.T.);
#2292=FACE_OUTER_BOUND('',#3279,.T.);
#2293=FACE_OUTER_BOUND('',#3280,.T.);
#2294=FACE_OUTER_BOUND('',#3281,.T.);
#2295=FACE_OUTER_BOUND('',#3282,.T.);
#2296=FACE_OUTER_BOUND('',#3283,.T.);
#2297=FACE_OUTER_BOUND('',#3284,.T.);
#2298=FACE_OUTER_BOUND('',#3285,.T.);
#2299=FACE_OUTER_BOUND('',#3286,.T.);
#2300=FACE_OUTER_BOUND('',#3287,.T.);
#2301=FACE_OUTER_BOUND('',#3288,.T.);
#2302=FACE_OUTER_BOUND('',#3289,.T.);
#2303=FACE_OUTER_BOUND('',#3290,.T.);
#2304=FACE_OUTER_BOUND('',#3291,.T.);
#2305=FACE_OUTER_BOUND('',#3292,.T.);
#2306=FACE_OUTER_BOUND('',#3293,.T.);
#2307=FACE_OUTER_BOUND('',#3294,.T.);
#2308=FACE_OUTER_BOUND('',#3295,.T.);
#2309=FACE_OUTER_BOUND('',#3296,.T.);
#2310=FACE_OUTER_BOUND('',#3297,.T.);
#2311=FACE_OUTER_BOUND('',#3298,.T.);
#2312=FACE_OUTER_BOUND('',#3299,.T.);
#2313=FACE_OUTER_BOUND('',#3302,.T.);
#2314=FACE_OUTER_BOUND('',#3303,.T.);
#2315=FACE_OUTER_BOUND('',#3304,.T.);
#2316=FACE_OUTER_BOUND('',#3305,.T.);
#2317=FACE_OUTER_BOUND('',#3306,.T.);
#2318=FACE_OUTER_BOUND('',#3307,.T.);
#2319=FACE_OUTER_BOUND('',#3308,.T.);
#2320=FACE_OUTER_BOUND('',#3309,.T.);
#2321=FACE_OUTER_BOUND('',#3310,.T.);
#2322=FACE_OUTER_BOUND('',#3311,.T.);
#2323=FACE_OUTER_BOUND('',#3312,.T.);
#2324=FACE_OUTER_BOUND('',#3313,.T.);
#2325=FACE_OUTER_BOUND('',#3314,.T.);
#2326=FACE_OUTER_BOUND('',#3315,.T.);
#2327=FACE_OUTER_BOUND('',#3316,.T.);
#2328=FACE_OUTER_BOUND('',#3317,.T.);
#2329=FACE_OUTER_BOUND('',#3318,.T.);
#2330=FACE_OUTER_BOUND('',#3319,.T.);
#2331=FACE_OUTER_BOUND('',#3320,.T.);
#2332=FACE_OUTER_BOUND('',#3322,.T.);
#2333=FACE_OUTER_BOUND('',#3323,.T.);
#2334=FACE_OUTER_BOUND('',#3324,.T.);
#2335=FACE_OUTER_BOUND('',#3325,.T.);
#2336=FACE_OUTER_BOUND('',#3326,.T.);
#2337=FACE_OUTER_BOUND('',#3327,.T.);
#2338=FACE_OUTER_BOUND('',#3328,.T.);
#2339=FACE_OUTER_BOUND('',#3332,.T.);
#2340=FACE_OUTER_BOUND('',#3333,.T.);
#2341=FACE_OUTER_BOUND('',#3334,.T.);
#2342=FACE_OUTER_BOUND('',#3335,.T.);
#2343=FACE_OUTER_BOUND('',#3337,.T.);
#2344=FACE_OUTER_BOUND('',#3338,.T.);
#2345=FACE_OUTER_BOUND('',#3339,.T.);
#2346=FACE_OUTER_BOUND('',#3340,.T.);
#2347=FACE_OUTER_BOUND('',#3341,.T.);
#2348=FACE_OUTER_BOUND('',#3342,.T.);
#2349=FACE_OUTER_BOUND('',#3343,.T.);
#2350=FACE_OUTER_BOUND('',#3344,.T.);
#2351=FACE_OUTER_BOUND('',#3345,.T.);
#2352=FACE_OUTER_BOUND('',#3346,.T.);
#2353=FACE_OUTER_BOUND('',#3347,.T.);
#2354=FACE_OUTER_BOUND('',#3348,.T.);
#2355=FACE_OUTER_BOUND('',#3349,.T.);
#2356=FACE_OUTER_BOUND('',#3350,.T.);
#2357=FACE_OUTER_BOUND('',#3351,.T.);
#2358=FACE_OUTER_BOUND('',#3352,.T.);
#2359=FACE_OUTER_BOUND('',#3353,.T.);
#2360=FACE_OUTER_BOUND('',#3354,.T.);
#2361=FACE_OUTER_BOUND('',#3355,.T.);
#2362=FACE_OUTER_BOUND('',#3356,.T.);
#2363=FACE_OUTER_BOUND('',#3357,.T.);
#2364=FACE_OUTER_BOUND('',#3358,.T.);
#2365=FACE_OUTER_BOUND('',#3359,.T.);
#2366=FACE_OUTER_BOUND('',#3360,.T.);
#2367=FACE_OUTER_BOUND('',#3361,.T.);
#2368=FACE_OUTER_BOUND('',#3362,.T.);
#2369=FACE_OUTER_BOUND('',#3363,.T.);
#2370=FACE_OUTER_BOUND('',#3364,.T.);
#2371=FACE_OUTER_BOUND('',#3365,.T.);
#2372=FACE_OUTER_BOUND('',#3366,.T.);
#2373=FACE_OUTER_BOUND('',#3367,.T.);
#2374=FACE_OUTER_BOUND('',#3368,.T.);
#2375=FACE_OUTER_BOUND('',#3369,.T.);
#2376=FACE_OUTER_BOUND('',#3370,.T.);
#2377=FACE_OUTER_BOUND('',#3371,.T.);
#2378=FACE_OUTER_BOUND('',#3372,.T.);
#2379=FACE_OUTER_BOUND('',#3373,.T.);
#2380=FACE_OUTER_BOUND('',#3374,.T.);
#2381=FACE_OUTER_BOUND('',#3375,.T.);
#2382=FACE_OUTER_BOUND('',#3376,.T.);
#2383=FACE_OUTER_BOUND('',#3377,.T.);
#2384=FACE_OUTER_BOUND('',#3378,.T.);
#2385=FACE_OUTER_BOUND('',#3379,.T.);
#2386=FACE_OUTER_BOUND('',#3380,.T.);
#2387=FACE_OUTER_BOUND('',#3381,.T.);
#2388=FACE_OUTER_BOUND('',#3382,.T.);
#2389=FACE_OUTER_BOUND('',#3383,.T.);
#2390=FACE_OUTER_BOUND('',#3384,.T.);
#2391=FACE_OUTER_BOUND('',#3385,.T.);
#2392=FACE_OUTER_BOUND('',#3386,.T.);
#2393=FACE_OUTER_BOUND('',#3387,.T.);
#2394=FACE_OUTER_BOUND('',#3388,.T.);
#2395=FACE_OUTER_BOUND('',#3389,.T.);
#2396=FACE_OUTER_BOUND('',#3390,.T.);
#2397=FACE_OUTER_BOUND('',#3391,.T.);
#2398=FACE_OUTER_BOUND('',#3392,.T.);
#2399=FACE_OUTER_BOUND('',#3393,.T.);
#2400=FACE_OUTER_BOUND('',#3394,.T.);
#2401=FACE_OUTER_BOUND('',#3395,.T.);
#2402=FACE_OUTER_BOUND('',#3396,.T.);
#2403=FACE_OUTER_BOUND('',#3397,.T.);
#2404=FACE_OUTER_BOUND('',#3398,.T.);
#2405=FACE_OUTER_BOUND('',#3399,.T.);
#2406=FACE_OUTER_BOUND('',#3400,.T.);
#2407=FACE_OUTER_BOUND('',#3401,.T.);
#2408=FACE_OUTER_BOUND('',#3402,.T.);
#2409=FACE_OUTER_BOUND('',#3403,.T.);
#2410=FACE_OUTER_BOUND('',#3404,.T.);
#2411=FACE_OUTER_BOUND('',#3405,.T.);
#2412=FACE_OUTER_BOUND('',#3406,.T.);
#2413=FACE_OUTER_BOUND('',#3407,.T.);
#2414=FACE_OUTER_BOUND('',#3409,.T.);
#2415=FACE_OUTER_BOUND('',#3410,.T.);
#2416=FACE_OUTER_BOUND('',#3411,.T.);
#2417=FACE_OUTER_BOUND('',#3412,.T.);
#2418=FACE_OUTER_BOUND('',#3413,.T.);
#2419=FACE_OUTER_BOUND('',#3414,.T.);
#2420=FACE_OUTER_BOUND('',#3415,.T.);
#2421=FACE_OUTER_BOUND('',#3416,.T.);
#2422=FACE_OUTER_BOUND('',#3417,.T.);
#2423=FACE_OUTER_BOUND('',#3418,.T.);
#2424=FACE_OUTER_BOUND('',#3419,.T.);
#2425=FACE_OUTER_BOUND('',#3420,.T.);
#2426=FACE_OUTER_BOUND('',#3421,.T.);
#2427=FACE_OUTER_BOUND('',#3422,.T.);
#2428=FACE_OUTER_BOUND('',#3423,.T.);
#2429=FACE_OUTER_BOUND('',#3424,.T.);
#2430=FACE_OUTER_BOUND('',#3425,.T.);
#2431=FACE_OUTER_BOUND('',#3426,.T.);
#2432=FACE_OUTER_BOUND('',#3427,.T.);
#2433=FACE_OUTER_BOUND('',#3428,.T.);
#2434=FACE_OUTER_BOUND('',#3429,.T.);
#2435=FACE_OUTER_BOUND('',#3430,.T.);
#2436=FACE_OUTER_BOUND('',#3431,.T.);
#2437=FACE_OUTER_BOUND('',#3432,.T.);
#2438=FACE_OUTER_BOUND('',#3433,.T.);
#2439=FACE_OUTER_BOUND('',#3434,.T.);
#2440=FACE_OUTER_BOUND('',#3435,.T.);
#2441=FACE_OUTER_BOUND('',#3436,.T.);
#2442=FACE_OUTER_BOUND('',#3437,.T.);
#2443=FACE_OUTER_BOUND('',#3438,.T.);
#2444=FACE_OUTER_BOUND('',#3439,.T.);
#2445=FACE_OUTER_BOUND('',#3440,.T.);
#2446=FACE_OUTER_BOUND('',#3441,.T.);
#2447=FACE_OUTER_BOUND('',#3442,.T.);
#2448=FACE_OUTER_BOUND('',#3443,.T.);
#2449=FACE_OUTER_BOUND('',#3444,.T.);
#2450=FACE_OUTER_BOUND('',#3445,.T.);
#2451=FACE_OUTER_BOUND('',#3446,.T.);
#2452=FACE_OUTER_BOUND('',#3447,.T.);
#2453=FACE_OUTER_BOUND('',#3448,.T.);
#2454=FACE_OUTER_BOUND('',#3449,.T.);
#2455=FACE_OUTER_BOUND('',#3450,.T.);
#2456=FACE_OUTER_BOUND('',#3451,.T.);
#2457=FACE_OUTER_BOUND('',#3452,.T.);
#2458=FACE_OUTER_BOUND('',#3453,.T.);
#2459=FACE_OUTER_BOUND('',#3454,.T.);
#2460=FACE_OUTER_BOUND('',#3455,.T.);
#2461=FACE_OUTER_BOUND('',#3456,.T.);
#2462=FACE_OUTER_BOUND('',#3457,.T.);
#2463=FACE_OUTER_BOUND('',#3458,.T.);
#2464=FACE_OUTER_BOUND('',#3459,.T.);
#2465=FACE_OUTER_BOUND('',#3460,.T.);
#2466=FACE_OUTER_BOUND('',#3461,.T.);
#2467=FACE_OUTER_BOUND('',#3462,.T.);
#2468=FACE_OUTER_BOUND('',#3463,.T.);
#2469=FACE_OUTER_BOUND('',#3464,.T.);
#2470=FACE_OUTER_BOUND('',#3465,.T.);
#2471=FACE_OUTER_BOUND('',#3466,.T.);
#2472=FACE_OUTER_BOUND('',#3467,.T.);
#2473=FACE_OUTER_BOUND('',#3468,.T.);
#2474=FACE_OUTER_BOUND('',#3469,.T.);
#2475=FACE_OUTER_BOUND('',#3470,.T.);
#2476=FACE_OUTER_BOUND('',#3471,.T.);
#2477=FACE_OUTER_BOUND('',#3472,.T.);
#2478=FACE_OUTER_BOUND('',#3473,.T.);
#2479=FACE_OUTER_BOUND('',#3474,.T.);
#2480=FACE_OUTER_BOUND('',#3475,.T.);
#2481=FACE_OUTER_BOUND('',#3476,.T.);
#2482=FACE_OUTER_BOUND('',#3477,.T.);
#2483=FACE_OUTER_BOUND('',#3478,.T.);
#2484=FACE_OUTER_BOUND('',#3479,.T.);
#2485=FACE_OUTER_BOUND('',#3480,.T.);
#2486=FACE_OUTER_BOUND('',#3481,.T.);
#2487=FACE_OUTER_BOUND('',#3482,.T.);
#2488=FACE_OUTER_BOUND('',#3483,.T.);
#2489=FACE_OUTER_BOUND('',#3484,.T.);
#2490=FACE_OUTER_BOUND('',#3485,.T.);
#2491=FACE_OUTER_BOUND('',#3486,.T.);
#2492=FACE_OUTER_BOUND('',#3487,.T.);
#2493=FACE_OUTER_BOUND('',#3488,.T.);
#2494=FACE_OUTER_BOUND('',#3489,.T.);
#2495=FACE_OUTER_BOUND('',#3490,.T.);
#2496=FACE_OUTER_BOUND('',#3491,.T.);
#2497=FACE_OUTER_BOUND('',#3492,.T.);
#2498=FACE_OUTER_BOUND('',#3493,.T.);
#2499=FACE_OUTER_BOUND('',#3494,.T.);
#2500=FACE_OUTER_BOUND('',#3495,.T.);
#2501=FACE_OUTER_BOUND('',#3496,.T.);
#2502=FACE_OUTER_BOUND('',#3497,.T.);
#2503=FACE_OUTER_BOUND('',#3498,.T.);
#2504=FACE_OUTER_BOUND('',#3499,.T.);
#2505=FACE_OUTER_BOUND('',#3500,.T.);
#2506=FACE_OUTER_BOUND('',#3501,.T.);
#2507=FACE_OUTER_BOUND('',#3502,.T.);
#2508=FACE_OUTER_BOUND('',#3503,.T.);
#2509=FACE_OUTER_BOUND('',#3504,.T.);
#2510=FACE_OUTER_BOUND('',#3505,.T.);
#2511=FACE_OUTER_BOUND('',#3506,.T.);
#2512=FACE_OUTER_BOUND('',#3507,.T.);
#2513=FACE_OUTER_BOUND('',#3508,.T.);
#2514=FACE_OUTER_BOUND('',#3509,.T.);
#2515=FACE_OUTER_BOUND('',#3510,.T.);
#2516=FACE_OUTER_BOUND('',#3511,.T.);
#2517=FACE_OUTER_BOUND('',#3512,.T.);
#2518=FACE_OUTER_BOUND('',#3513,.T.);
#2519=FACE_OUTER_BOUND('',#3514,.T.);
#2520=FACE_OUTER_BOUND('',#3515,.T.);
#2521=FACE_OUTER_BOUND('',#3516,.T.);
#2522=FACE_OUTER_BOUND('',#3517,.T.);
#2523=FACE_OUTER_BOUND('',#3518,.T.);
#2524=FACE_OUTER_BOUND('',#3519,.T.);
#2525=FACE_OUTER_BOUND('',#3520,.T.);
#2526=FACE_OUTER_BOUND('',#3521,.T.);
#2527=FACE_OUTER_BOUND('',#3522,.T.);
#2528=FACE_OUTER_BOUND('',#3523,.T.);
#2529=FACE_OUTER_BOUND('',#3524,.T.);
#2530=FACE_OUTER_BOUND('',#3525,.T.);
#2531=FACE_OUTER_BOUND('',#3526,.T.);
#2532=FACE_OUTER_BOUND('',#3527,.T.);
#2533=FACE_OUTER_BOUND('',#3528,.T.);
#2534=FACE_OUTER_BOUND('',#3529,.T.);
#2535=FACE_OUTER_BOUND('',#3530,.T.);
#2536=FACE_OUTER_BOUND('',#3531,.T.);
#2537=FACE_OUTER_BOUND('',#3532,.T.);
#2538=FACE_OUTER_BOUND('',#3533,.T.);
#2539=FACE_OUTER_BOUND('',#3534,.T.);
#2540=FACE_OUTER_BOUND('',#3535,.T.);
#2541=FACE_OUTER_BOUND('',#3536,.T.);
#2542=FACE_OUTER_BOUND('',#3537,.T.);
#2543=FACE_OUTER_BOUND('',#3538,.T.);
#2544=FACE_OUTER_BOUND('',#3539,.T.);
#2545=FACE_OUTER_BOUND('',#3540,.T.);
#2546=FACE_OUTER_BOUND('',#3541,.T.);
#2547=FACE_OUTER_BOUND('',#3542,.T.);
#2548=FACE_OUTER_BOUND('',#3543,.T.);
#2549=FACE_OUTER_BOUND('',#3544,.T.);
#2550=FACE_OUTER_BOUND('',#3545,.T.);
#2551=FACE_OUTER_BOUND('',#3546,.T.);
#2552=FACE_OUTER_BOUND('',#3547,.T.);
#2553=FACE_OUTER_BOUND('',#3548,.T.);
#2554=FACE_OUTER_BOUND('',#3549,.T.);
#2555=FACE_OUTER_BOUND('',#3550,.T.);
#2556=FACE_OUTER_BOUND('',#3551,.T.);
#2557=FACE_OUTER_BOUND('',#3552,.T.);
#2558=FACE_OUTER_BOUND('',#3553,.T.);
#2559=FACE_OUTER_BOUND('',#3554,.T.);
#2560=FACE_OUTER_BOUND('',#3555,.T.);
#2561=FACE_OUTER_BOUND('',#3556,.T.);
#2562=FACE_OUTER_BOUND('',#3557,.T.);
#2563=FACE_OUTER_BOUND('',#3558,.T.);
#2564=FACE_OUTER_BOUND('',#3559,.T.);
#2565=FACE_OUTER_BOUND('',#3560,.T.);
#2566=FACE_OUTER_BOUND('',#3561,.T.);
#2567=FACE_OUTER_BOUND('',#3562,.T.);
#2568=FACE_OUTER_BOUND('',#3563,.T.);
#2569=FACE_OUTER_BOUND('',#3564,.T.);
#2570=FACE_OUTER_BOUND('',#3565,.T.);
#2571=FACE_OUTER_BOUND('',#3566,.T.);
#2572=FACE_OUTER_BOUND('',#3567,.T.);
#2573=FACE_OUTER_BOUND('',#3568,.T.);
#2574=FACE_OUTER_BOUND('',#3569,.T.);
#2575=FACE_OUTER_BOUND('',#3570,.T.);
#2576=FACE_OUTER_BOUND('',#3571,.T.);
#2577=FACE_OUTER_BOUND('',#3572,.T.);
#2578=FACE_OUTER_BOUND('',#3573,.T.);
#2579=FACE_OUTER_BOUND('',#3574,.T.);
#2580=FACE_OUTER_BOUND('',#3575,.T.);
#2581=FACE_OUTER_BOUND('',#3576,.T.);
#2582=FACE_OUTER_BOUND('',#3577,.T.);
#2583=FACE_OUTER_BOUND('',#3578,.T.);
#2584=FACE_OUTER_BOUND('',#3579,.T.);
#2585=FACE_OUTER_BOUND('',#3580,.T.);
#2586=FACE_OUTER_BOUND('',#3581,.T.);
#2587=FACE_OUTER_BOUND('',#3582,.T.);
#2588=FACE_OUTER_BOUND('',#3583,.T.);
#2589=FACE_OUTER_BOUND('',#3584,.T.);
#2590=FACE_OUTER_BOUND('',#3585,.T.);
#2591=FACE_OUTER_BOUND('',#3586,.T.);
#2592=FACE_OUTER_BOUND('',#3587,.T.);
#2593=FACE_OUTER_BOUND('',#3588,.T.);
#2594=FACE_OUTER_BOUND('',#3589,.T.);
#2595=FACE_OUTER_BOUND('',#3590,.T.);
#2596=FACE_OUTER_BOUND('',#3591,.T.);
#2597=FACE_OUTER_BOUND('',#3592,.T.);
#2598=FACE_OUTER_BOUND('',#3593,.T.);
#2599=FACE_OUTER_BOUND('',#3594,.T.);
#2600=FACE_OUTER_BOUND('',#3595,.T.);
#2601=FACE_OUTER_BOUND('',#3596,.T.);
#2602=FACE_OUTER_BOUND('',#3597,.T.);
#2603=FACE_OUTER_BOUND('',#3598,.T.);
#2604=FACE_OUTER_BOUND('',#3599,.T.);
#2605=FACE_OUTER_BOUND('',#3600,.T.);
#2606=FACE_OUTER_BOUND('',#3601,.T.);
#2607=FACE_OUTER_BOUND('',#3602,.T.);
#2608=FACE_OUTER_BOUND('',#3603,.T.);
#2609=FACE_OUTER_BOUND('',#3604,.T.);
#2610=FACE_OUTER_BOUND('',#3605,.T.);
#2611=FACE_OUTER_BOUND('',#3606,.T.);
#2612=FACE_OUTER_BOUND('',#3607,.T.);
#2613=FACE_OUTER_BOUND('',#3608,.T.);
#2614=FACE_OUTER_BOUND('',#3609,.T.);
#2615=FACE_OUTER_BOUND('',#3610,.T.);
#2616=FACE_OUTER_BOUND('',#3611,.T.);
#2617=FACE_OUTER_BOUND('',#3612,.T.);
#2618=FACE_OUTER_BOUND('',#3613,.T.);
#2619=FACE_OUTER_BOUND('',#3614,.T.);
#2620=FACE_OUTER_BOUND('',#3615,.T.);
#2621=FACE_OUTER_BOUND('',#3616,.T.);
#2622=FACE_OUTER_BOUND('',#3617,.T.);
#2623=FACE_OUTER_BOUND('',#3618,.T.);
#2624=FACE_OUTER_BOUND('',#3619,.T.);
#2625=FACE_OUTER_BOUND('',#3620,.T.);
#2626=FACE_OUTER_BOUND('',#3621,.T.);
#2627=FACE_OUTER_BOUND('',#3622,.T.);
#2628=FACE_OUTER_BOUND('',#3623,.T.);
#2629=FACE_OUTER_BOUND('',#3624,.T.);
#2630=FACE_OUTER_BOUND('',#3625,.T.);
#2631=FACE_OUTER_BOUND('',#3626,.T.);
#2632=FACE_OUTER_BOUND('',#3627,.T.);
#2633=FACE_OUTER_BOUND('',#3628,.T.);
#2634=FACE_OUTER_BOUND('',#3629,.T.);
#2635=FACE_OUTER_BOUND('',#3630,.T.);
#2636=FACE_OUTER_BOUND('',#3631,.T.);
#2637=FACE_OUTER_BOUND('',#3632,.T.);
#2638=FACE_OUTER_BOUND('',#3633,.T.);
#2639=FACE_OUTER_BOUND('',#3634,.T.);
#2640=FACE_OUTER_BOUND('',#3635,.T.);
#2641=FACE_OUTER_BOUND('',#3636,.T.);
#2642=FACE_OUTER_BOUND('',#3637,.T.);
#2643=FACE_OUTER_BOUND('',#3638,.T.);
#2644=FACE_OUTER_BOUND('',#3639,.T.);
#2645=FACE_OUTER_BOUND('',#3640,.T.);
#2646=FACE_OUTER_BOUND('',#3641,.T.);
#2647=FACE_OUTER_BOUND('',#3642,.T.);
#2648=FACE_OUTER_BOUND('',#3643,.T.);
#2649=FACE_OUTER_BOUND('',#3644,.T.);
#2650=FACE_OUTER_BOUND('',#3645,.T.);
#2651=FACE_OUTER_BOUND('',#3646,.T.);
#2652=FACE_OUTER_BOUND('',#3647,.T.);
#2653=FACE_OUTER_BOUND('',#3648,.T.);
#2654=FACE_OUTER_BOUND('',#3649,.T.);
#2655=FACE_OUTER_BOUND('',#3650,.T.);
#2656=FACE_OUTER_BOUND('',#3651,.T.);
#2657=FACE_OUTER_BOUND('',#3652,.T.);
#2658=FACE_OUTER_BOUND('',#3653,.T.);
#2659=FACE_OUTER_BOUND('',#3654,.T.);
#2660=FACE_OUTER_BOUND('',#3655,.T.);
#2661=FACE_OUTER_BOUND('',#3656,.T.);
#2662=FACE_OUTER_BOUND('',#3657,.T.);
#2663=FACE_OUTER_BOUND('',#3658,.T.);
#2664=FACE_OUTER_BOUND('',#3659,.T.);
#2665=FACE_OUTER_BOUND('',#3660,.T.);
#2666=FACE_OUTER_BOUND('',#3661,.T.);
#2667=FACE_OUTER_BOUND('',#3662,.T.);
#2668=FACE_OUTER_BOUND('',#3663,.T.);
#2669=FACE_OUTER_BOUND('',#3664,.T.);
#2670=FACE_OUTER_BOUND('',#3665,.T.);
#2671=FACE_OUTER_BOUND('',#3666,.T.);
#2672=FACE_OUTER_BOUND('',#3667,.T.);
#2673=FACE_OUTER_BOUND('',#3668,.T.);
#2674=FACE_OUTER_BOUND('',#3669,.T.);
#2675=FACE_OUTER_BOUND('',#3670,.T.);
#2676=FACE_OUTER_BOUND('',#3671,.T.);
#2677=FACE_OUTER_BOUND('',#3672,.T.);
#2678=FACE_OUTER_BOUND('',#3673,.T.);
#2679=FACE_OUTER_BOUND('',#3674,.T.);
#2680=FACE_OUTER_BOUND('',#3675,.T.);
#2681=FACE_OUTER_BOUND('',#3676,.T.);
#2682=FACE_OUTER_BOUND('',#3677,.T.);
#2683=FACE_OUTER_BOUND('',#3678,.T.);
#2684=FACE_OUTER_BOUND('',#3679,.T.);
#2685=FACE_OUTER_BOUND('',#3680,.T.);
#2686=FACE_OUTER_BOUND('',#3681,.T.);
#2687=FACE_OUTER_BOUND('',#3682,.T.);
#2688=FACE_OUTER_BOUND('',#3683,.T.);
#2689=FACE_OUTER_BOUND('',#3684,.T.);
#2690=FACE_OUTER_BOUND('',#3685,.T.);
#2691=FACE_OUTER_BOUND('',#3686,.T.);
#2692=FACE_OUTER_BOUND('',#3687,.T.);
#2693=FACE_OUTER_BOUND('',#3688,.T.);
#2694=FACE_OUTER_BOUND('',#3689,.T.);
#2695=FACE_OUTER_BOUND('',#3690,.T.);
#2696=FACE_OUTER_BOUND('',#3691,.T.);
#2697=FACE_OUTER_BOUND('',#3692,.T.);
#2698=FACE_OUTER_BOUND('',#3693,.T.);
#2699=FACE_OUTER_BOUND('',#3694,.T.);
#2700=FACE_OUTER_BOUND('',#3695,.T.);
#2701=FACE_OUTER_BOUND('',#3696,.T.);
#2702=FACE_OUTER_BOUND('',#3697,.T.);
#2703=FACE_OUTER_BOUND('',#3698,.T.);
#2704=FACE_OUTER_BOUND('',#3699,.T.);
#2705=FACE_OUTER_BOUND('',#3700,.T.);
#2706=FACE_OUTER_BOUND('',#3701,.T.);
#2707=FACE_OUTER_BOUND('',#3702,.T.);
#2708=FACE_OUTER_BOUND('',#3703,.T.);
#2709=FACE_OUTER_BOUND('',#3704,.T.);
#2710=FACE_OUTER_BOUND('',#3705,.T.);
#2711=FACE_OUTER_BOUND('',#3706,.T.);
#2712=FACE_OUTER_BOUND('',#3707,.T.);
#2713=FACE_OUTER_BOUND('',#3708,.T.);
#2714=FACE_OUTER_BOUND('',#3709,.T.);
#2715=FACE_OUTER_BOUND('',#3710,.T.);
#2716=FACE_OUTER_BOUND('',#3711,.T.);
#2717=FACE_OUTER_BOUND('',#3712,.T.);
#2718=FACE_OUTER_BOUND('',#3713,.T.);
#2719=FACE_OUTER_BOUND('',#3714,.T.);
#2720=FACE_OUTER_BOUND('',#3715,.T.);
#2721=FACE_OUTER_BOUND('',#3716,.T.);
#2722=FACE_OUTER_BOUND('',#3717,.T.);
#2723=FACE_OUTER_BOUND('',#3718,.T.);
#2724=FACE_OUTER_BOUND('',#3719,.T.);
#2725=FACE_OUTER_BOUND('',#3720,.T.);
#2726=FACE_OUTER_BOUND('',#3721,.T.);
#2727=FACE_OUTER_BOUND('',#3722,.T.);
#2728=FACE_OUTER_BOUND('',#3723,.T.);
#2729=FACE_OUTER_BOUND('',#3724,.T.);
#2730=FACE_OUTER_BOUND('',#3725,.T.);
#2731=FACE_OUTER_BOUND('',#3726,.T.);
#2732=FACE_OUTER_BOUND('',#3727,.T.);
#2733=FACE_OUTER_BOUND('',#3728,.T.);
#2734=FACE_OUTER_BOUND('',#3729,.T.);
#2735=FACE_OUTER_BOUND('',#3730,.T.);
#2736=FACE_OUTER_BOUND('',#3731,.T.);
#2737=FACE_OUTER_BOUND('',#3732,.T.);
#2738=FACE_OUTER_BOUND('',#3733,.T.);
#2739=FACE_OUTER_BOUND('',#3734,.T.);
#2740=FACE_OUTER_BOUND('',#3735,.T.);
#2741=FACE_OUTER_BOUND('',#3736,.T.);
#2742=FACE_OUTER_BOUND('',#3737,.T.);
#2743=FACE_OUTER_BOUND('',#3738,.T.);
#2744=FACE_OUTER_BOUND('',#3739,.T.);
#2745=FACE_OUTER_BOUND('',#3740,.T.);
#2746=FACE_OUTER_BOUND('',#3741,.T.);
#2747=FACE_OUTER_BOUND('',#3742,.T.);
#2748=FACE_OUTER_BOUND('',#3743,.T.);
#2749=FACE_OUTER_BOUND('',#3744,.T.);
#2750=FACE_OUTER_BOUND('',#3745,.T.);
#2751=FACE_OUTER_BOUND('',#3746,.T.);
#2752=FACE_OUTER_BOUND('',#3747,.T.);
#2753=FACE_OUTER_BOUND('',#3748,.T.);
#2754=FACE_OUTER_BOUND('',#3749,.T.);
#2755=FACE_OUTER_BOUND('',#3750,.T.);
#2756=FACE_OUTER_BOUND('',#3751,.T.);
#2757=FACE_OUTER_BOUND('',#3752,.T.);
#2758=FACE_OUTER_BOUND('',#3753,.T.);
#2759=FACE_OUTER_BOUND('',#3754,.T.);
#2760=FACE_OUTER_BOUND('',#3755,.T.);
#2761=FACE_OUTER_BOUND('',#3756,.T.);
#2762=FACE_OUTER_BOUND('',#3757,.T.);
#2763=FACE_OUTER_BOUND('',#3758,.T.);
#2764=FACE_OUTER_BOUND('',#3759,.T.);
#2765=FACE_OUTER_BOUND('',#3760,.T.);
#2766=FACE_OUTER_BOUND('',#3761,.T.);
#2767=FACE_OUTER_BOUND('',#3762,.T.);
#2768=FACE_OUTER_BOUND('',#3763,.T.);
#2769=FACE_OUTER_BOUND('',#3764,.T.);
#2770=FACE_OUTER_BOUND('',#3765,.T.);
#2771=FACE_OUTER_BOUND('',#3766,.T.);
#2772=FACE_OUTER_BOUND('',#3767,.T.);
#2773=FACE_OUTER_BOUND('',#3768,.T.);
#2774=FACE_OUTER_BOUND('',#3769,.T.);
#2775=FACE_OUTER_BOUND('',#3770,.T.);
#2776=FACE_OUTER_BOUND('',#3771,.T.);
#2777=FACE_OUTER_BOUND('',#3772,.T.);
#2778=FACE_OUTER_BOUND('',#3773,.T.);
#2779=FACE_OUTER_BOUND('',#3774,.T.);
#2780=FACE_OUTER_BOUND('',#3775,.T.);
#2781=FACE_OUTER_BOUND('',#3776,.T.);
#2782=FACE_OUTER_BOUND('',#3777,.T.);
#2783=FACE_OUTER_BOUND('',#3778,.T.);
#2784=FACE_OUTER_BOUND('',#3779,.T.);
#2785=FACE_OUTER_BOUND('',#3780,.T.);
#2786=FACE_OUTER_BOUND('',#3781,.T.);
#2787=FACE_OUTER_BOUND('',#3782,.T.);
#2788=FACE_OUTER_BOUND('',#3783,.T.);
#2789=FACE_OUTER_BOUND('',#3784,.T.);
#2790=FACE_OUTER_BOUND('',#3785,.T.);
#2791=FACE_OUTER_BOUND('',#3786,.T.);
#2792=FACE_OUTER_BOUND('',#3787,.T.);
#2793=FACE_OUTER_BOUND('',#3788,.T.);
#2794=FACE_OUTER_BOUND('',#3789,.T.);
#2795=FACE_OUTER_BOUND('',#3790,.T.);
#2796=FACE_OUTER_BOUND('',#3791,.T.);
#2797=FACE_OUTER_BOUND('',#3792,.T.);
#2798=FACE_OUTER_BOUND('',#3793,.T.);
#2799=FACE_OUTER_BOUND('',#3794,.T.);
#2800=FACE_OUTER_BOUND('',#3795,.T.);
#2801=FACE_OUTER_BOUND('',#3796,.T.);
#2802=FACE_OUTER_BOUND('',#3797,.T.);
#2803=FACE_OUTER_BOUND('',#3798,.T.);
#2804=FACE_OUTER_BOUND('',#3799,.T.);
#2805=FACE_OUTER_BOUND('',#3800,.T.);
#2806=FACE_OUTER_BOUND('',#3801,.T.);
#2807=FACE_OUTER_BOUND('',#3802,.T.);
#2808=FACE_OUTER_BOUND('',#3803,.T.);
#2809=FACE_OUTER_BOUND('',#3804,.T.);
#2810=FACE_OUTER_BOUND('',#3805,.T.);
#2811=FACE_OUTER_BOUND('',#3806,.T.);
#2812=FACE_OUTER_BOUND('',#3807,.T.);
#2813=FACE_OUTER_BOUND('',#3808,.T.);
#2814=FACE_OUTER_BOUND('',#3809,.T.);
#2815=FACE_OUTER_BOUND('',#3810,.T.);
#2816=FACE_OUTER_BOUND('',#3811,.T.);
#2817=FACE_OUTER_BOUND('',#3812,.T.);
#2818=FACE_OUTER_BOUND('',#3813,.T.);
#2819=FACE_OUTER_BOUND('',#3814,.T.);
#2820=FACE_OUTER_BOUND('',#3815,.T.);
#2821=FACE_OUTER_BOUND('',#3816,.T.);
#2822=FACE_OUTER_BOUND('',#3817,.T.);
#2823=FACE_OUTER_BOUND('',#3818,.T.);
#2824=FACE_OUTER_BOUND('',#3819,.T.);
#2825=FACE_OUTER_BOUND('',#3820,.T.);
#2826=FACE_OUTER_BOUND('',#3821,.T.);
#2827=FACE_OUTER_BOUND('',#3822,.T.);
#2828=FACE_OUTER_BOUND('',#3823,.T.);
#2829=FACE_OUTER_BOUND('',#3824,.T.);
#2830=FACE_OUTER_BOUND('',#3825,.T.);
#2831=FACE_OUTER_BOUND('',#3826,.T.);
#2832=FACE_OUTER_BOUND('',#3827,.T.);
#2833=FACE_OUTER_BOUND('',#3828,.T.);
#2834=FACE_OUTER_BOUND('',#3829,.T.);
#2835=FACE_OUTER_BOUND('',#3830,.T.);
#2836=FACE_OUTER_BOUND('',#3831,.T.);
#2837=FACE_OUTER_BOUND('',#3832,.T.);
#2838=FACE_OUTER_BOUND('',#3833,.T.);
#2839=FACE_OUTER_BOUND('',#3834,.T.);
#2840=FACE_OUTER_BOUND('',#3835,.T.);
#2841=FACE_OUTER_BOUND('',#3836,.T.);
#2842=FACE_OUTER_BOUND('',#3837,.T.);
#2843=FACE_OUTER_BOUND('',#3838,.T.);
#2844=FACE_OUTER_BOUND('',#3839,.T.);
#2845=FACE_OUTER_BOUND('',#3840,.T.);
#2846=FACE_OUTER_BOUND('',#3841,.T.);
#2847=FACE_OUTER_BOUND('',#3842,.T.);
#2848=FACE_OUTER_BOUND('',#3843,.T.);
#2849=FACE_OUTER_BOUND('',#3844,.T.);
#2850=FACE_OUTER_BOUND('',#3845,.T.);
#2851=FACE_OUTER_BOUND('',#3846,.T.);
#2852=FACE_OUTER_BOUND('',#3847,.T.);
#2853=FACE_OUTER_BOUND('',#3848,.T.);
#2854=FACE_OUTER_BOUND('',#3849,.T.);
#2855=FACE_OUTER_BOUND('',#3850,.T.);
#2856=FACE_OUTER_BOUND('',#3851,.T.);
#2857=FACE_OUTER_BOUND('',#3852,.T.);
#2858=FACE_OUTER_BOUND('',#3853,.T.);
#2859=FACE_OUTER_BOUND('',#3854,.T.);
#2860=FACE_OUTER_BOUND('',#3856,.T.);
#2861=FACE_OUTER_BOUND('',#3857,.T.);
#2862=FACE_OUTER_BOUND('',#3858,.T.);
#2863=FACE_OUTER_BOUND('',#3865,.T.);
#2864=FACE_OUTER_BOUND('',#3866,.T.);
#2865=FACE_OUTER_BOUND('',#3867,.T.);
#2866=FACE_OUTER_BOUND('',#3868,.T.);
#2867=FACE_OUTER_BOUND('',#3869,.T.);
#2868=FACE_OUTER_BOUND('',#3870,.T.);
#2869=FACE_OUTER_BOUND('',#3871,.T.);
#2870=FACE_OUTER_BOUND('',#3872,.T.);
#2871=FACE_OUTER_BOUND('',#3873,.T.);
#2872=FACE_OUTER_BOUND('',#3874,.T.);
#2873=FACE_OUTER_BOUND('',#3875,.T.);
#2874=FACE_OUTER_BOUND('',#3876,.T.);
#2875=FACE_OUTER_BOUND('',#3877,.T.);
#2876=FACE_OUTER_BOUND('',#3878,.T.);
#2877=FACE_OUTER_BOUND('',#3879,.T.);
#2878=FACE_OUTER_BOUND('',#3880,.T.);
#2879=FACE_OUTER_BOUND('',#3881,.T.);
#2880=FACE_OUTER_BOUND('',#3882,.T.);
#2881=FACE_OUTER_BOUND('',#3883,.T.);
#2882=FACE_OUTER_BOUND('',#3884,.T.);
#2883=FACE_OUTER_BOUND('',#3885,.T.);
#2884=FACE_OUTER_BOUND('',#3886,.T.);
#2885=FACE_OUTER_BOUND('',#3887,.T.);
#2886=FACE_OUTER_BOUND('',#3888,.T.);
#2887=FACE_OUTER_BOUND('',#3889,.T.);
#2888=FACE_OUTER_BOUND('',#3890,.T.);
#2889=FACE_OUTER_BOUND('',#3891,.T.);
#2890=FACE_OUTER_BOUND('',#3892,.T.);
#2891=FACE_OUTER_BOUND('',#3893,.T.);
#2892=FACE_OUTER_BOUND('',#3894,.T.);
#2893=FACE_OUTER_BOUND('',#3895,.T.);
#2894=FACE_OUTER_BOUND('',#3896,.T.);
#2895=FACE_OUTER_BOUND('',#3897,.T.);
#2896=FACE_OUTER_BOUND('',#3898,.T.);
#2897=FACE_OUTER_BOUND('',#3899,.T.);
#2898=FACE_OUTER_BOUND('',#3900,.T.);
#2899=FACE_OUTER_BOUND('',#3901,.T.);
#2900=FACE_OUTER_BOUND('',#3902,.T.);
#2901=FACE_OUTER_BOUND('',#3903,.T.);
#2902=FACE_OUTER_BOUND('',#3904,.T.);
#2903=FACE_OUTER_BOUND('',#3905,.T.);
#2904=FACE_OUTER_BOUND('',#3906,.T.);
#2905=FACE_OUTER_BOUND('',#3907,.T.);
#2906=FACE_OUTER_BOUND('',#3908,.T.);
#2907=FACE_OUTER_BOUND('',#3909,.T.);
#2908=FACE_OUTER_BOUND('',#3910,.T.);
#2909=FACE_OUTER_BOUND('',#3911,.T.);
#2910=FACE_OUTER_BOUND('',#3912,.T.);
#2911=FACE_OUTER_BOUND('',#3913,.T.);
#2912=FACE_OUTER_BOUND('',#3914,.T.);
#2913=FACE_OUTER_BOUND('',#3915,.T.);
#2914=FACE_OUTER_BOUND('',#3916,.T.);
#2915=FACE_OUTER_BOUND('',#3917,.T.);
#2916=FACE_OUTER_BOUND('',#3918,.T.);
#2917=FACE_OUTER_BOUND('',#3919,.T.);
#2918=FACE_OUTER_BOUND('',#3920,.T.);
#2919=FACE_OUTER_BOUND('',#3921,.T.);
#2920=FACE_OUTER_BOUND('',#3922,.T.);
#2921=FACE_OUTER_BOUND('',#3923,.T.);
#2922=FACE_OUTER_BOUND('',#3924,.T.);
#2923=FACE_OUTER_BOUND('',#3925,.T.);
#2924=FACE_OUTER_BOUND('',#3926,.T.);
#2925=FACE_OUTER_BOUND('',#3927,.T.);
#2926=FACE_OUTER_BOUND('',#3928,.T.);
#2927=FACE_OUTER_BOUND('',#3929,.T.);
#2928=FACE_OUTER_BOUND('',#3930,.T.);
#2929=FACE_OUTER_BOUND('',#3931,.T.);
#2930=FACE_OUTER_BOUND('',#3932,.T.);
#2931=FACE_OUTER_BOUND('',#3933,.T.);
#2932=FACE_OUTER_BOUND('',#3934,.T.);
#2933=FACE_OUTER_BOUND('',#3935,.T.);
#2934=FACE_OUTER_BOUND('',#3936,.T.);
#2935=FACE_OUTER_BOUND('',#3937,.T.);
#2936=FACE_OUTER_BOUND('',#3938,.T.);
#2937=FACE_OUTER_BOUND('',#3939,.T.);
#2938=FACE_OUTER_BOUND('',#3940,.T.);
#2939=FACE_OUTER_BOUND('',#3941,.T.);
#2940=FACE_OUTER_BOUND('',#3942,.T.);
#2941=FACE_OUTER_BOUND('',#3943,.T.);
#2942=FACE_OUTER_BOUND('',#3944,.T.);
#2943=FACE_OUTER_BOUND('',#3945,.T.);
#2944=FACE_OUTER_BOUND('',#3946,.T.);
#2945=FACE_OUTER_BOUND('',#3947,.T.);
#2946=FACE_OUTER_BOUND('',#3948,.T.);
#2947=FACE_OUTER_BOUND('',#3949,.T.);
#2948=FACE_OUTER_BOUND('',#3950,.T.);
#2949=FACE_OUTER_BOUND('',#3951,.T.);
#2950=FACE_OUTER_BOUND('',#3952,.T.);
#2951=FACE_OUTER_BOUND('',#3953,.T.);
#2952=FACE_OUTER_BOUND('',#3954,.T.);
#2953=FACE_OUTER_BOUND('',#3955,.T.);
#2954=FACE_OUTER_BOUND('',#3956,.T.);
#2955=FACE_OUTER_BOUND('',#3957,.T.);
#2956=FACE_OUTER_BOUND('',#3958,.T.);
#2957=FACE_OUTER_BOUND('',#3959,.T.);
#2958=FACE_OUTER_BOUND('',#3960,.T.);
#2959=FACE_OUTER_BOUND('',#3961,.T.);
#2960=FACE_OUTER_BOUND('',#3962,.T.);
#2961=FACE_OUTER_BOUND('',#3963,.T.);
#2962=FACE_OUTER_BOUND('',#3964,.T.);
#2963=FACE_OUTER_BOUND('',#3965,.T.);
#2964=FACE_OUTER_BOUND('',#3966,.T.);
#2965=FACE_OUTER_BOUND('',#3967,.T.);
#2966=FACE_OUTER_BOUND('',#3968,.T.);
#2967=FACE_OUTER_BOUND('',#3969,.T.);
#2968=FACE_OUTER_BOUND('',#3970,.T.);
#2969=FACE_OUTER_BOUND('',#3971,.T.);
#2970=FACE_OUTER_BOUND('',#3972,.T.);
#2971=FACE_OUTER_BOUND('',#3973,.T.);
#2972=FACE_OUTER_BOUND('',#3974,.T.);
#2973=FACE_OUTER_BOUND('',#3975,.T.);
#2974=FACE_OUTER_BOUND('',#3976,.T.);
#2975=FACE_OUTER_BOUND('',#3977,.T.);
#2976=FACE_OUTER_BOUND('',#3978,.T.);
#2977=FACE_OUTER_BOUND('',#3979,.T.);
#2978=FACE_OUTER_BOUND('',#3980,.T.);
#2979=FACE_OUTER_BOUND('',#3981,.T.);
#2980=FACE_OUTER_BOUND('',#3982,.T.);
#2981=FACE_OUTER_BOUND('',#3983,.T.);
#2982=FACE_OUTER_BOUND('',#3984,.T.);
#2983=FACE_OUTER_BOUND('',#3985,.T.);
#2984=FACE_OUTER_BOUND('',#3986,.T.);
#2985=FACE_OUTER_BOUND('',#3987,.T.);
#2986=FACE_OUTER_BOUND('',#3988,.T.);
#2987=FACE_OUTER_BOUND('',#4000,.T.);
#2988=FACE_OUTER_BOUND('',#4001,.T.);
#2989=FACE_OUTER_BOUND('',#4002,.T.);
#2990=FACE_OUTER_BOUND('',#4003,.T.);
#2991=FACE_OUTER_BOUND('',#4004,.T.);
#2992=FACE_OUTER_BOUND('',#4005,.T.);
#2993=FACE_OUTER_BOUND('',#4006,.T.);
#2994=FACE_OUTER_BOUND('',#4007,.T.);
#2995=FACE_OUTER_BOUND('',#4008,.T.);
#2996=FACE_OUTER_BOUND('',#4009,.T.);
#2997=FACE_OUTER_BOUND('',#4010,.T.);
#2998=FACE_OUTER_BOUND('',#4011,.T.);
#2999=FACE_OUTER_BOUND('',#4012,.T.);
#3000=FACE_OUTER_BOUND('',#4013,.T.);
#3001=FACE_OUTER_BOUND('',#4014,.T.);
#3002=FACE_OUTER_BOUND('',#4015,.T.);
#3003=FACE_OUTER_BOUND('',#4016,.T.);
#3004=FACE_OUTER_BOUND('',#4017,.T.);
#3005=FACE_OUTER_BOUND('',#4018,.T.);
#3006=FACE_OUTER_BOUND('',#4019,.T.);
#3007=FACE_OUTER_BOUND('',#4020,.T.);
#3008=FACE_OUTER_BOUND('',#4021,.T.);
#3009=FACE_OUTER_BOUND('',#4022,.T.);
#3010=FACE_OUTER_BOUND('',#4023,.T.);
#3011=FACE_OUTER_BOUND('',#4024,.T.);
#3012=FACE_OUTER_BOUND('',#4025,.T.);
#3013=FACE_OUTER_BOUND('',#4026,.T.);
#3014=FACE_OUTER_BOUND('',#4027,.T.);
#3015=FACE_OUTER_BOUND('',#4029,.T.);
#3016=FACE_OUTER_BOUND('',#4030,.T.);
#3017=FACE_OUTER_BOUND('',#4031,.T.);
#3018=FACE_OUTER_BOUND('',#4033,.T.);
#3019=FACE_OUTER_BOUND('',#4034,.T.);
#3020=FACE_OUTER_BOUND('',#4035,.T.);
#3021=FACE_OUTER_BOUND('',#4037,.T.);
#3022=FACE_OUTER_BOUND('',#4038,.T.);
#3023=FACE_OUTER_BOUND('',#4039,.T.);
#3024=FACE_OUTER_BOUND('',#4040,.T.);
#3025=FACE_OUTER_BOUND('',#4041,.T.);
#3026=FACE_OUTER_BOUND('',#4042,.T.);
#3027=FACE_OUTER_BOUND('',#4043,.T.);
#3028=FACE_OUTER_BOUND('',#4044,.T.);
#3029=FACE_OUTER_BOUND('',#4045,.T.);
#3030=FACE_OUTER_BOUND('',#4046,.T.);
#3031=FACE_OUTER_BOUND('',#4047,.T.);
#3032=FACE_OUTER_BOUND('',#4048,.T.);
#3033=FACE_OUTER_BOUND('',#4049,.T.);
#3034=FACE_OUTER_BOUND('',#4050,.T.);
#3035=FACE_OUTER_BOUND('',#4051,.T.);
#3036=FACE_OUTER_BOUND('',#4052,.T.);
#3037=FACE_OUTER_BOUND('',#4053,.T.);
#3038=FACE_OUTER_BOUND('',#4054,.T.);
#3039=FACE_OUTER_BOUND('',#4055,.T.);
#3040=FACE_OUTER_BOUND('',#4056,.T.);
#3041=FACE_OUTER_BOUND('',#4057,.T.);
#3042=FACE_OUTER_BOUND('',#4059,.T.);
#3043=FACE_OUTER_BOUND('',#4060,.T.);
#3044=FACE_OUTER_BOUND('',#4061,.T.);
#3045=FACE_OUTER_BOUND('',#4062,.T.);
#3046=FACE_OUTER_BOUND('',#4063,.T.);
#3047=FACE_OUTER_BOUND('',#4064,.T.);
#3048=FACE_OUTER_BOUND('',#4066,.T.);
#3049=FACE_OUTER_BOUND('',#4067,.T.);
#3050=FACE_OUTER_BOUND('',#4068,.T.);
#3051=FACE_OUTER_BOUND('',#4069,.T.);
#3052=FACE_OUTER_BOUND('',#4070,.T.);
#3053=FACE_OUTER_BOUND('',#4072,.T.);
#3054=FACE_OUTER_BOUND('',#4073,.T.);
#3055=FACE_OUTER_BOUND('',#4075,.T.);
#3056=FACE_OUTER_BOUND('',#4076,.T.);
#3057=FACE_OUTER_BOUND('',#4077,.T.);
#3058=FACE_OUTER_BOUND('',#4079,.T.);
#3059=FACE_OUTER_BOUND('',#4080,.T.);
#3060=FACE_OUTER_BOUND('',#4082,.T.);
#3061=FACE_OUTER_BOUND('',#4083,.T.);
#3062=FACE_OUTER_BOUND('',#4084,.T.);
#3063=FACE_OUTER_BOUND('',#4086,.T.);
#3064=FACE_OUTER_BOUND('',#4087,.T.);
#3065=FACE_OUTER_BOUND('',#4089,.T.);
#3066=FACE_OUTER_BOUND('',#4090,.T.);
#3067=FACE_OUTER_BOUND('',#4091,.T.);
#3068=FACE_OUTER_BOUND('',#4092,.T.);
#3069=FACE_OUTER_BOUND('',#4094,.T.);
#3070=FACE_OUTER_BOUND('',#4095,.T.);
#3071=FACE_OUTER_BOUND('',#4097,.T.);
#3072=FACE_OUTER_BOUND('',#4098,.T.);
#3073=FACE_OUTER_BOUND('',#4099,.T.);
#3074=FACE_OUTER_BOUND('',#4100,.T.);
#3075=FACE_OUTER_BOUND('',#4101,.T.);
#3076=FACE_OUTER_BOUND('',#4102,.T.);
#3077=FACE_OUTER_BOUND('',#4103,.T.);
#3078=FACE_OUTER_BOUND('',#4104,.T.);
#3079=FACE_OUTER_BOUND('',#4105,.T.);
#3080=FACE_OUTER_BOUND('',#4106,.T.);
#3081=FACE_OUTER_BOUND('',#4107,.T.);
#3082=FACE_OUTER_BOUND('',#4108,.T.);
#3083=FACE_OUTER_BOUND('',#4109,.T.);
#3084=FACE_OUTER_BOUND('',#4110,.T.);
#3085=FACE_OUTER_BOUND('',#4111,.T.);
#3086=FACE_OUTER_BOUND('',#4112,.T.);
#3087=FACE_OUTER_BOUND('',#4113,.T.);
#3088=FACE_OUTER_BOUND('',#4114,.T.);
#3089=FACE_OUTER_BOUND('',#4115,.T.);
#3090=FACE_OUTER_BOUND('',#4116,.T.);
#3091=FACE_OUTER_BOUND('',#4117,.T.);
#3092=FACE_OUTER_BOUND('',#4118,.T.);
#3093=FACE_OUTER_BOUND('',#4119,.T.);
#3094=FACE_OUTER_BOUND('',#4120,.T.);
#3095=FACE_OUTER_BOUND('',#4121,.T.);
#3096=FACE_OUTER_BOUND('',#4122,.T.);
#3097=FACE_OUTER_BOUND('',#4123,.T.);
#3098=FACE_OUTER_BOUND('',#4124,.T.);
#3099=FACE_OUTER_BOUND('',#4125,.T.);
#3100=FACE_OUTER_BOUND('',#4126,.T.);
#3101=FACE_OUTER_BOUND('',#4127,.T.);
#3102=FACE_OUTER_BOUND('',#4128,.T.);
#3103=FACE_OUTER_BOUND('',#4129,.T.);
#3104=FACE_OUTER_BOUND('',#4130,.T.);
#3105=FACE_OUTER_BOUND('',#4131,.T.);
#3106=FACE_OUTER_BOUND('',#4132,.T.);
#3107=FACE_OUTER_BOUND('',#4133,.T.);
#3108=FACE_OUTER_BOUND('',#4134,.T.);
#3109=FACE_OUTER_BOUND('',#4135,.T.);
#3110=FACE_OUTER_BOUND('',#4136,.T.);
#3111=FACE_OUTER_BOUND('',#4137,.T.);
#3112=FACE_OUTER_BOUND('',#4138,.T.);
#3113=FACE_OUTER_BOUND('',#4139,.T.);
#3114=FACE_OUTER_BOUND('',#4140,.T.);
#3115=FACE_OUTER_BOUND('',#4141,.T.);
#3116=FACE_OUTER_BOUND('',#4142,.T.);
#3117=FACE_OUTER_BOUND('',#4143,.T.);
#3118=FACE_OUTER_BOUND('',#4144,.T.);
#3119=FACE_OUTER_BOUND('',#4145,.T.);
#3120=FACE_OUTER_BOUND('',#4146,.T.);
#3121=FACE_OUTER_BOUND('',#4147,.T.);
#3122=FACE_OUTER_BOUND('',#4148,.T.);
#3123=FACE_OUTER_BOUND('',#4149,.T.);
#3124=FACE_OUTER_BOUND('',#4150,.T.);
#3125=FACE_OUTER_BOUND('',#4151,.T.);
#3126=FACE_OUTER_BOUND('',#4152,.T.);
#3127=FACE_OUTER_BOUND('',#4153,.T.);
#3128=FACE_OUTER_BOUND('',#4154,.T.);
#3129=FACE_OUTER_BOUND('',#4155,.T.);
#3130=FACE_OUTER_BOUND('',#4156,.T.);
#3131=FACE_OUTER_BOUND('',#4157,.T.);
#3132=FACE_OUTER_BOUND('',#4159,.T.);
#3133=FACE_OUTER_BOUND('',#4160,.T.);
#3134=FACE_OUTER_BOUND('',#4161,.T.);
#3135=FACE_OUTER_BOUND('',#4162,.T.);
#3136=FACE_OUTER_BOUND('',#4163,.T.);
#3137=FACE_OUTER_BOUND('',#4164,.T.);
#3138=FACE_OUTER_BOUND('',#4165,.T.);
#3139=FACE_OUTER_BOUND('',#4166,.T.);
#3140=FACE_OUTER_BOUND('',#4167,.T.);
#3141=FACE_OUTER_BOUND('',#4168,.T.);
#3142=FACE_OUTER_BOUND('',#4169,.T.);
#3143=FACE_OUTER_BOUND('',#4170,.T.);
#3144=FACE_OUTER_BOUND('',#4171,.T.);
#3145=FACE_OUTER_BOUND('',#4172,.T.);
#3146=FACE_OUTER_BOUND('',#4173,.T.);
#3147=FACE_OUTER_BOUND('',#4174,.T.);
#3148=FACE_OUTER_BOUND('',#4175,.T.);
#3149=FACE_OUTER_BOUND('',#4176,.T.);
#3150=FACE_OUTER_BOUND('',#4177,.T.);
#3151=FACE_OUTER_BOUND('',#4178,.T.);
#3152=FACE_OUTER_BOUND('',#4179,.T.);
#3153=FACE_OUTER_BOUND('',#4180,.T.);
#3154=FACE_OUTER_BOUND('',#4181,.T.);
#3155=FACE_OUTER_BOUND('',#4182,.T.);
#3156=FACE_OUTER_BOUND('',#4183,.T.);
#3157=FACE_OUTER_BOUND('',#4184,.T.);
#3158=FACE_OUTER_BOUND('',#4185,.T.);
#3159=FACE_OUTER_BOUND('',#4186,.T.);
#3160=FACE_OUTER_BOUND('',#4187,.T.);
#3161=FACE_OUTER_BOUND('',#4188,.T.);
#3162=FACE_OUTER_BOUND('',#4189,.T.);
#3163=FACE_OUTER_BOUND('',#4190,.T.);
#3164=FACE_OUTER_BOUND('',#4191,.T.);
#3165=FACE_OUTER_BOUND('',#4192,.T.);
#3166=FACE_OUTER_BOUND('',#4193,.T.);
#3167=FACE_OUTER_BOUND('',#4194,.T.);
#3168=FACE_OUTER_BOUND('',#4195,.T.);
#3169=FACE_OUTER_BOUND('',#4196,.T.);
#3170=FACE_OUTER_BOUND('',#4197,.T.);
#3171=FACE_OUTER_BOUND('',#4198,.T.);
#3172=FACE_OUTER_BOUND('',#4199,.T.);
#3173=FACE_OUTER_BOUND('',#4200,.T.);
#3174=FACE_OUTER_BOUND('',#4201,.T.);
#3175=FACE_OUTER_BOUND('',#4202,.T.);
#3176=FACE_OUTER_BOUND('',#4203,.T.);
#3177=FACE_OUTER_BOUND('',#4204,.T.);
#3178=FACE_OUTER_BOUND('',#4205,.T.);
#3179=FACE_OUTER_BOUND('',#4206,.T.);
#3180=FACE_OUTER_BOUND('',#4207,.T.);
#3181=FACE_OUTER_BOUND('',#4208,.T.);
#3182=FACE_OUTER_BOUND('',#4209,.T.);
#3183=FACE_OUTER_BOUND('',#4210,.T.);
#3184=FACE_OUTER_BOUND('',#4211,.T.);
#3185=FACE_OUTER_BOUND('',#4212,.T.);
#3186=FACE_OUTER_BOUND('',#4213,.T.);
#3187=FACE_OUTER_BOUND('',#4214,.T.);
#3188=FACE_OUTER_BOUND('',#4215,.T.);
#3189=FACE_OUTER_BOUND('',#4216,.T.);
#3190=FACE_OUTER_BOUND('',#4217,.T.);
#3191=FACE_OUTER_BOUND('',#4218,.T.);
#3192=FACE_OUTER_BOUND('',#4219,.T.);
#3193=FACE_OUTER_BOUND('',#4220,.T.);
#3194=FACE_OUTER_BOUND('',#4221,.T.);
#3195=FACE_OUTER_BOUND('',#4222,.T.);
#3196=FACE_OUTER_BOUND('',#4223,.T.);
#3197=FACE_OUTER_BOUND('',#4224,.T.);
#3198=FACE_OUTER_BOUND('',#4225,.T.);
#3199=FACE_OUTER_BOUND('',#4226,.T.);
#3200=FACE_OUTER_BOUND('',#4227,.T.);
#3201=FACE_OUTER_BOUND('',#4228,.T.);
#3202=FACE_OUTER_BOUND('',#4229,.T.);
#3203=FACE_OUTER_BOUND('',#4230,.T.);
#3204=FACE_OUTER_BOUND('',#4231,.T.);
#3205=FACE_OUTER_BOUND('',#4232,.T.);
#3206=FACE_OUTER_BOUND('',#4233,.T.);
#3207=FACE_OUTER_BOUND('',#4234,.T.);
#3208=FACE_OUTER_BOUND('',#4235,.T.);
#3209=FACE_OUTER_BOUND('',#4236,.T.);
#3210=FACE_OUTER_BOUND('',#4237,.T.);
#3211=FACE_OUTER_BOUND('',#4238,.T.);
#3212=FACE_OUTER_BOUND('',#4239,.T.);
#3213=FACE_OUTER_BOUND('',#4240,.T.);
#3214=FACE_OUTER_BOUND('',#4241,.T.);
#3215=FACE_OUTER_BOUND('',#4242,.T.);
#3216=FACE_OUTER_BOUND('',#4243,.T.);
#3217=FACE_OUTER_BOUND('',#4244,.T.);
#3218=FACE_OUTER_BOUND('',#4245,.T.);
#3219=FACE_OUTER_BOUND('',#4246,.T.);
#3220=FACE_OUTER_BOUND('',#4247,.T.);
#3221=FACE_OUTER_BOUND('',#4248,.T.);
#3222=FACE_OUTER_BOUND('',#4249,.T.);
#3223=FACE_OUTER_BOUND('',#4250,.T.);
#3224=FACE_OUTER_BOUND('',#4251,.T.);
#3225=FACE_OUTER_BOUND('',#4252,.T.);
#3226=FACE_OUTER_BOUND('',#4253,.T.);
#3227=FACE_OUTER_BOUND('',#4254,.T.);
#3228=FACE_OUTER_BOUND('',#4255,.T.);
#3229=FACE_OUTER_BOUND('',#4256,.T.);
#3230=FACE_OUTER_BOUND('',#4257,.T.);
#3231=FACE_OUTER_BOUND('',#4258,.T.);
#3232=FACE_OUTER_BOUND('',#4259,.T.);
#3233=FACE_OUTER_BOUND('',#4260,.T.);
#3234=FACE_OUTER_BOUND('',#4261,.T.);
#3235=FACE_OUTER_BOUND('',#4262,.T.);
#3236=FACE_OUTER_BOUND('',#4263,.T.);
#3237=FACE_OUTER_BOUND('',#4264,.T.);
#3238=FACE_OUTER_BOUND('',#4265,.T.);
#3239=FACE_OUTER_BOUND('',#4266,.T.);
#3240=FACE_OUTER_BOUND('',#4267,.T.);
#3241=FACE_OUTER_BOUND('',#4268,.T.);
#3242=FACE_OUTER_BOUND('',#4269,.T.);
#3243=FACE_OUTER_BOUND('',#4270,.T.);
#3244=FACE_OUTER_BOUND('',#4271,.T.);
#3245=FACE_OUTER_BOUND('',#4272,.T.);
#3246=FACE_OUTER_BOUND('',#4273,.T.);
#3247=FACE_OUTER_BOUND('',#4274,.T.);
#3248=FACE_OUTER_BOUND('',#4275,.T.);
#3249=FACE_OUTER_BOUND('',#4276,.T.);
#3250=FACE_OUTER_BOUND('',#4277,.T.);
#3251=FACE_OUTER_BOUND('',#4278,.T.);
#3252=FACE_OUTER_BOUND('',#4279,.T.);
#3253=FACE_OUTER_BOUND('',#4280,.T.);
#3254=FACE_OUTER_BOUND('',#4281,.T.);
#3255=FACE_OUTER_BOUND('',#4282,.T.);
#3256=FACE_OUTER_BOUND('',#4283,.T.);
#3257=FACE_OUTER_BOUND('',#4284,.T.);
#3258=FACE_OUTER_BOUND('',#4285,.T.);
#3259=FACE_OUTER_BOUND('',#4286,.T.);
#3260=FACE_OUTER_BOUND('',#4288,.T.);
#3261=FACE_OUTER_BOUND('',#4289,.T.);
#3262=FACE_OUTER_BOUND('',#4290,.T.);
#3263=EDGE_LOOP('',(#10459,#10460,#10461,#10462));
#3264=EDGE_LOOP('',(#10463,#10464,#10465,#10466));
#3265=EDGE_LOOP('',(#10467,#10468,#10469,#10470));
#3266=EDGE_LOOP('',(#10471,#10472,#10473,#10474));
#3267=EDGE_LOOP('',(#10475,#10476,#10477,#10478));
#3268=EDGE_LOOP('',(#10479,#10480,#10481,#10482));
#3269=EDGE_LOOP('',(#10483,#10484,#10485,#10486,#10487));
#3270=EDGE_LOOP('',(#10488,#10489,#10490,#10491));
#3271=EDGE_LOOP('',(#10492,#10493,#10494,#10495));
#3272=EDGE_LOOP('',(#10496,#10497,#10498,#10499));
#3273=EDGE_LOOP('',(#10500,#10501,#10502,#10503));
#3274=EDGE_LOOP('',(#10504,#10505,#10506,#10507));
#3275=EDGE_LOOP('',(#10508,#10509,#10510,#10511));
#3276=EDGE_LOOP('',(#10512,#10513,#10514,#10515));
#3277=EDGE_LOOP('',(#10516,#10517,#10518,#10519));
#3278=EDGE_LOOP('',(#10520,#10521,#10522,#10523));
#3279=EDGE_LOOP('',(#10524,#10525,#10526,#10527));
#3280=EDGE_LOOP('',(#10528,#10529,#10530,#10531));
#3281=EDGE_LOOP('',(#10532,#10533,#10534,#10535));
#3282=EDGE_LOOP('',(#10536,#10537,#10538,#10539));
#3283=EDGE_LOOP('',(#10540,#10541,#10542,#10543));
#3284=EDGE_LOOP('',(#10544,#10545,#10546,#10547));
#3285=EDGE_LOOP('',(#10548,#10549,#10550,#10551));
#3286=EDGE_LOOP('',(#10552,#10553,#10554,#10555));
#3287=EDGE_LOOP('',(#10556,#10557,#10558,#10559));
#3288=EDGE_LOOP('',(#10560,#10561,#10562));
#3289=EDGE_LOOP('',(#10563,#10564,#10565,#10566));
#3290=EDGE_LOOP('',(#10567,#10568,#10569));
#3291=EDGE_LOOP('',(#10570,#10571,#10572,#10573));
#3292=EDGE_LOOP('',(#10574,#10575,#10576,#10577,#10578));
#3293=EDGE_LOOP('',(#10579,#10580,#10581,#10582));
#3294=EDGE_LOOP('',(#10583,#10584,#10585,#10586,#10587));
#3295=EDGE_LOOP('',(#10588,#10589,#10590,#10591,#10592));
#3296=EDGE_LOOP('',(#10593,#10594,#10595,#10596,#10597));
#3297=EDGE_LOOP('',(#10598,#10599,#10600,#10601,#10602));
#3298=EDGE_LOOP('',(#10603,#10604,#10605,#10606,#10607,#10608,#10609,#10610));
#3299=EDGE_LOOP('',(#10611,#10612,#10613,#10614,#10615,#10616,#10617,#10618));
#3300=EDGE_LOOP('',(#10619));
#3301=EDGE_LOOP('',(#10620));
#3302=EDGE_LOOP('',(#10621,#10622,#10623,#10624,#10625));
#3303=EDGE_LOOP('',(#10626,#10627,#10628,#10629));
#3304=EDGE_LOOP('',(#10630,#10631,#10632,#10633));
#3305=EDGE_LOOP('',(#10634,#10635,#10636,#10637));
#3306=EDGE_LOOP('',(#10638,#10639,#10640,#10641));
#3307=EDGE_LOOP('',(#10642,#10643,#10644,#10645));
#3308=EDGE_LOOP('',(#10646,#10647,#10648,#10649));
#3309=EDGE_LOOP('',(#10650,#10651,#10652,#10653));
#3310=EDGE_LOOP('',(#10654,#10655,#10656,#10657));
#3311=EDGE_LOOP('',(#10658,#10659,#10660,#10661));
#3312=EDGE_LOOP('',(#10662,#10663,#10664,#10665));
#3313=EDGE_LOOP('',(#10666,#10667,#10668,#10669));
#3314=EDGE_LOOP('',(#10670,#10671,#10672,#10673));
#3315=EDGE_LOOP('',(#10674,#10675,#10676,#10677,#10678));
#3316=EDGE_LOOP('',(#10679,#10680,#10681,#10682,#10683));
#3317=EDGE_LOOP('',(#10684,#10685,#10686,#10687,#10688,#10689));
#3318=EDGE_LOOP('',(#10690,#10691,#10692,#10693));
#3319=EDGE_LOOP('',(#10694,#10695,#10696,#10697));
#3320=EDGE_LOOP('',(#10698,#10699));
#3321=EDGE_LOOP('',(#10700));
#3322=EDGE_LOOP('',(#10701,#10702,#10703,#10704));
#3323=EDGE_LOOP('',(#10705,#10706,#10707,#10708));
#3324=EDGE_LOOP('',(#10709,#10710,#10711,#10712,#10713,#10714,#10715,#10716,
#10717,#10718,#10719,#10720));
#3325=EDGE_LOOP('',(#10721,#10722,#10723,#10724));
#3326=EDGE_LOOP('',(#10725,#10726,#10727,#10728));
#3327=EDGE_LOOP('',(#10729,#10730,#10731,#10732));
#3328=EDGE_LOOP('',(#10733));
#3329=EDGE_LOOP('',(#10734));
#3330=EDGE_LOOP('',(#10735));
#3331=EDGE_LOOP('',(#10736));
#3332=EDGE_LOOP('',(#10737,#10738,#10739,#10740));
#3333=EDGE_LOOP('',(#10741,#10742,#10743,#10744));
#3334=EDGE_LOOP('',(#10745));
#3335=EDGE_LOOP('',(#10746));
#3336=EDGE_LOOP('',(#10747));
#3337=EDGE_LOOP('',(#10748,#10749,#10750,#10751));
#3338=EDGE_LOOP('',(#10752,#10753,#10754,#10755));
#3339=EDGE_LOOP('',(#10756));
#3340=EDGE_LOOP('',(#10757,#10758,#10759,#10760));
#3341=EDGE_LOOP('',(#10761,#10762,#10763,#10764));
#3342=EDGE_LOOP('',(#10765,#10766,#10767,#10768));
#3343=EDGE_LOOP('',(#10769,#10770,#10771,#10772));
#3344=EDGE_LOOP('',(#10773,#10774,#10775,#10776));
#3345=EDGE_LOOP('',(#10777,#10778,#10779,#10780));
#3346=EDGE_LOOP('',(#10781,#10782,#10783,#10784));
#3347=EDGE_LOOP('',(#10785,#10786,#10787,#10788));
#3348=EDGE_LOOP('',(#10789,#10790,#10791,#10792,#10793,#10794));
#3349=EDGE_LOOP('',(#10795,#10796,#10797,#10798,#10799));
#3350=EDGE_LOOP('',(#10800,#10801,#10802,#10803));
#3351=EDGE_LOOP('',(#10804,#10805,#10806,#10807,#10808,#10809));
#3352=EDGE_LOOP('',(#10810,#10811,#10812,#10813));
#3353=EDGE_LOOP('',(#10814,#10815,#10816,#10817,#10818,#10819));
#3354=EDGE_LOOP('',(#10820,#10821,#10822,#10823,#10824));
#3355=EDGE_LOOP('',(#10825,#10826,#10827,#10828,#10829,#10830));
#3356=EDGE_LOOP('',(#10831,#10832,#10833,#10834));
#3357=EDGE_LOOP('',(#10835,#10836,#10837,#10838,#10839));
#3358=EDGE_LOOP('',(#10840,#10841,#10842,#10843));
#3359=EDGE_LOOP('',(#10844,#10845,#10846,#10847,#10848,#10849));
#3360=EDGE_LOOP('',(#10850,#10851,#10852,#10853,#10854));
#3361=EDGE_LOOP('',(#10855,#10856,#10857,#10858,#10859,#10860));
#3362=EDGE_LOOP('',(#10861,#10862,#10863,#10864));
#3363=EDGE_LOOP('',(#10865,#10866,#10867,#10868,#10869));
#3364=EDGE_LOOP('',(#10870,#10871,#10872,#10873,#10874));
#3365=EDGE_LOOP('',(#10875,#10876,#10877,#10878));
#3366=EDGE_LOOP('',(#10879,#10880,#10881,#10882,#10883,#10884));
#3367=EDGE_LOOP('',(#10885,#10886,#10887,#10888,#10889,#10890));
#3368=EDGE_LOOP('',(#10891,#10892,#10893,#10894,#10895));
#3369=EDGE_LOOP('',(#10896,#10897,#10898,#10899));
#3370=EDGE_LOOP('',(#10900,#10901,#10902,#10903,#10904,#10905));
#3371=EDGE_LOOP('',(#10906,#10907,#10908,#10909,#10910));
#3372=EDGE_LOOP('',(#10911,#10912,#10913,#10914,#10915,#10916));
#3373=EDGE_LOOP('',(#10917,#10918,#10919,#10920));
#3374=EDGE_LOOP('',(#10921,#10922,#10923,#10924,#10925));
#3375=EDGE_LOOP('',(#10926,#10927,#10928,#10929,#10930));
#3376=EDGE_LOOP('',(#10931,#10932,#10933,#10934,#10935,#10936));
#3377=EDGE_LOOP('',(#10937,#10938,#10939,#10940));
#3378=EDGE_LOOP('',(#10941,#10942,#10943,#10944,#10945));
#3379=EDGE_LOOP('',(#10946,#10947,#10948,#10949,#10950));
#3380=EDGE_LOOP('',(#10951,#10952,#10953,#10954,#10955,#10956));
#3381=EDGE_LOOP('',(#10957,#10958,#10959,#10960));
#3382=EDGE_LOOP('',(#10961,#10962,#10963,#10964,#10965));
#3383=EDGE_LOOP('',(#10966,#10967,#10968,#10969,#10970));
#3384=EDGE_LOOP('',(#10971,#10972,#10973,#10974,#10975,#10976));
#3385=EDGE_LOOP('',(#10977,#10978,#10979,#10980));
#3386=EDGE_LOOP('',(#10981,#10982,#10983,#10984,#10985));
#3387=EDGE_LOOP('',(#10986,#10987,#10988,#10989,#10990));
#3388=EDGE_LOOP('',(#10991,#10992,#10993,#10994,#10995,#10996));
#3389=EDGE_LOOP('',(#10997,#10998,#10999,#11000));
#3390=EDGE_LOOP('',(#11001,#11002,#11003,#11004,#11005));
#3391=EDGE_LOOP('',(#11006,#11007,#11008,#11009,#11010));
#3392=EDGE_LOOP('',(#11011,#11012,#11013,#11014,#11015,#11016));
#3393=EDGE_LOOP('',(#11017,#11018,#11019,#11020));
#3394=EDGE_LOOP('',(#11021,#11022,#11023,#11024,#11025));
#3395=EDGE_LOOP('',(#11026,#11027,#11028,#11029,#11030));
#3396=EDGE_LOOP('',(#11031,#11032,#11033,#11034,#11035,#11036));
#3397=EDGE_LOOP('',(#11037,#11038,#11039,#11040));
#3398=EDGE_LOOP('',(#11041,#11042,#11043,#11044,#11045));
#3399=EDGE_LOOP('',(#11046,#11047,#11048,#11049,#11050));
#3400=EDGE_LOOP('',(#11051,#11052,#11053,#11054,#11055,#11056));
#3401=EDGE_LOOP('',(#11057,#11058,#11059,#11060));
#3402=EDGE_LOOP('',(#11061,#11062,#11063,#11064,#11065));
#3403=EDGE_LOOP('',(#11066,#11067,#11068,#11069,#11070,#11071));
#3404=EDGE_LOOP('',(#11072,#11073,#11074,#11075,#11076,#11077));
#3405=EDGE_LOOP('',(#11078,#11079,#11080,#11081,#11082,#11083));
#3406=EDGE_LOOP('',(#11084,#11085,#11086,#11087,#11088,#11089));
#3407=EDGE_LOOP('',(#11090,#11091,#11092,#11093,#11094,#11095,#11096,#11097,
#11098,#11099,#11100,#11101,#11102,#11103,#11104,#11105,#11106,#11107,#11108,
#11109,#11110,#11111,#11112,#11113,#11114,#11115,#11116,#11117,#11118,#11119,
#11120,#11121,#11122,#11123,#11124,#11125,#11126,#11127,#11128,#11129,#11130,
#11131,#11132,#11133,#11134,#11135,#11136,#11137,#11138,#11139,#11140,#11141,
#11142,#11143,#11144,#11145,#11146,#11147,#11148,#11149,#11150,#11151,#11152,
#11153,#11154,#11155,#11156,#11157,#11158,#11159,#11160,#11161,#11162,#11163,
#11164,#11165,#11166,#11167,#11168,#11169,#11170,#11171,#11172,#11173,#11174,
#11175,#11176,#11177,#11178,#11179,#11180,#11181,#11182,#11183,#11184,#11185,
#11186,#11187,#11188,#11189,#11190,#11191,#11192,#11193,#11194,#11195,#11196,
#11197,#11198,#11199,#11200,#11201,#11202,#11203,#11204,#11205,#11206,#11207,
#11208,#11209,#11210,#11211,#11212,#11213,#11214,#11215,#11216,#11217,#11218,
#11219,#11220,#11221,#11222,#11223,#11224,#11225,#11226,#11227,#11228,#11229,
#11230,#11231,#11232,#11233,#11234,#11235,#11236,#11237,#11238,#11239,#11240,
#11241,#11242,#11243,#11244,#11245,#11246,#11247,#11248,#11249,#11250,#11251,
#11252,#11253,#11254,#11255,#11256,#11257,#11258,#11259,#11260,#11261,#11262,
#11263,#11264,#11265,#11266,#11267,#11268,#11269));
#3408=EDGE_LOOP('',(#11270));
#3409=EDGE_LOOP('',(#11271,#11272,#11273,#11274,#11275,#11276));
#3410=EDGE_LOOP('',(#11277,#11278,#11279,#11280));
#3411=EDGE_LOOP('',(#11281,#11282,#11283,#11284,#11285));
#3412=EDGE_LOOP('',(#11286,#11287,#11288,#11289,#11290,#11291));
#3413=EDGE_LOOP('',(#11292,#11293,#11294,#11295));
#3414=EDGE_LOOP('',(#11296,#11297,#11298,#11299,#11300));
#3415=EDGE_LOOP('',(#11301,#11302,#11303,#11304,#11305));
#3416=EDGE_LOOP('',(#11306,#11307,#11308,#11309,#11310,#11311));
#3417=EDGE_LOOP('',(#11312,#11313,#11314,#11315));
#3418=EDGE_LOOP('',(#11316,#11317,#11318,#11319,#11320));
#3419=EDGE_LOOP('',(#11321,#11322,#11323,#11324,#11325));
#3420=EDGE_LOOP('',(#11326,#11327,#11328,#11329,#11330,#11331));
#3421=EDGE_LOOP('',(#11332,#11333,#11334,#11335));
#3422=EDGE_LOOP('',(#11336,#11337,#11338,#11339));
#3423=EDGE_LOOP('',(#11340,#11341,#11342,#11343));
#3424=EDGE_LOOP('',(#11344,#11345,#11346,#11347,#11348,#11349));
#3425=EDGE_LOOP('',(#11350,#11351,#11352,#11353,#11354));
#3426=EDGE_LOOP('',(#11355,#11356,#11357,#11358));
#3427=EDGE_LOOP('',(#11359,#11360,#11361,#11362,#11363,#11364));
#3428=EDGE_LOOP('',(#11365,#11366,#11367,#11368));
#3429=EDGE_LOOP('',(#11369,#11370,#11371,#11372,#11373));
#3430=EDGE_LOOP('',(#11374,#11375,#11376,#11377,#11378));
#3431=EDGE_LOOP('',(#11379,#11380,#11381,#11382,#11383,#11384));
#3432=EDGE_LOOP('',(#11385,#11386,#11387,#11388));
#3433=EDGE_LOOP('',(#11389,#11390,#11391,#11392,#11393));
#3434=EDGE_LOOP('',(#11394,#11395,#11396,#11397,#11398));
#3435=EDGE_LOOP('',(#11399,#11400,#11401,#11402,#11403,#11404));
#3436=EDGE_LOOP('',(#11405,#11406,#11407,#11408));
#3437=EDGE_LOOP('',(#11409,#11410,#11411,#11412,#11413));
#3438=EDGE_LOOP('',(#11414,#11415,#11416,#11417,#11418));
#3439=EDGE_LOOP('',(#11419,#11420,#11421,#11422,#11423,#11424));
#3440=EDGE_LOOP('',(#11425,#11426,#11427,#11428));
#3441=EDGE_LOOP('',(#11429,#11430,#11431,#11432,#11433));
#3442=EDGE_LOOP('',(#11434,#11435,#11436,#11437,#11438));
#3443=EDGE_LOOP('',(#11439,#11440,#11441,#11442,#11443,#11444));
#3444=EDGE_LOOP('',(#11445,#11446,#11447,#11448));
#3445=EDGE_LOOP('',(#11449,#11450,#11451,#11452,#11453));
#3446=EDGE_LOOP('',(#11454,#11455,#11456,#11457,#11458));
#3447=EDGE_LOOP('',(#11459,#11460,#11461,#11462,#11463,#11464));
#3448=EDGE_LOOP('',(#11465,#11466,#11467,#11468));
#3449=EDGE_LOOP('',(#11469,#11470,#11471,#11472));
#3450=EDGE_LOOP('',(#11473,#11474,#11475,#11476,#11477,#11478));
#3451=EDGE_LOOP('',(#11479,#11480,#11481,#11482,#11483,#11484));
#3452=EDGE_LOOP('',(#11485,#11486,#11487,#11488,#11489,#11490));
#3453=EDGE_LOOP('',(#11491,#11492,#11493,#11494));
#3454=EDGE_LOOP('',(#11495,#11496,#11497,#11498));
#3455=EDGE_LOOP('',(#11499,#11500,#11501,#11502));
#3456=EDGE_LOOP('',(#11503,#11504,#11505,#11506));
#3457=EDGE_LOOP('',(#11507,#11508,#11509,#11510,#11511,#11512));
#3458=EDGE_LOOP('',(#11513,#11514,#11515,#11516,#11517,#11518));
#3459=EDGE_LOOP('',(#11519,#11520,#11521,#11522,#11523,#11524));
#3460=EDGE_LOOP('',(#11525,#11526,#11527,#11528,#11529,#11530));
#3461=EDGE_LOOP('',(#11531,#11532,#11533,#11534,#11535,#11536));
#3462=EDGE_LOOP('',(#11537,#11538,#11539,#11540,#11541,#11542));
#3463=EDGE_LOOP('',(#11543,#11544,#11545,#11546));
#3464=EDGE_LOOP('',(#11547,#11548,#11549,#11550));
#3465=EDGE_LOOP('',(#11551,#11552,#11553,#11554));
#3466=EDGE_LOOP('',(#11555,#11556,#11557,#11558));
#3467=EDGE_LOOP('',(#11559,#11560,#11561,#11562));
#3468=EDGE_LOOP('',(#11563,#11564,#11565,#11566,#11567));
#3469=EDGE_LOOP('',(#11568,#11569,#11570,#11571,#11572,#11573));
#3470=EDGE_LOOP('',(#11574,#11575,#11576,#11577));
#3471=EDGE_LOOP('',(#11578,#11579,#11580,#11581,#11582));
#3472=EDGE_LOOP('',(#11583,#11584,#11585,#11586,#11587,#11588));
#3473=EDGE_LOOP('',(#11589,#11590,#11591,#11592,#11593));
#3474=EDGE_LOOP('',(#11594,#11595,#11596,#11597,#11598,#11599));
#3475=EDGE_LOOP('',(#11600,#11601,#11602,#11603));
#3476=EDGE_LOOP('',(#11604,#11605,#11606,#11607,#11608));
#3477=EDGE_LOOP('',(#11609,#11610,#11611,#11612,#11613));
#3478=EDGE_LOOP('',(#11614,#11615,#11616,#11617,#11618,#11619));
#3479=EDGE_LOOP('',(#11620,#11621,#11622,#11623));
#3480=EDGE_LOOP('',(#11624,#11625,#11626,#11627,#11628));
#3481=EDGE_LOOP('',(#11629,#11630,#11631,#11632,#11633));
#3482=EDGE_LOOP('',(#11634,#11635,#11636,#11637,#11638,#11639));
#3483=EDGE_LOOP('',(#11640,#11641,#11642,#11643));
#3484=EDGE_LOOP('',(#11644,#11645,#11646,#11647));
#3485=EDGE_LOOP('',(#11648,#11649,#11650,#11651));
#3486=EDGE_LOOP('',(#11652,#11653,#11654,#11655,#11656,#11657));
#3487=EDGE_LOOP('',(#11658,#11659,#11660,#11661,#11662));
#3488=EDGE_LOOP('',(#11663,#11664,#11665,#11666));
#3489=EDGE_LOOP('',(#11667,#11668,#11669,#11670,#11671,#11672));
#3490=EDGE_LOOP('',(#11673,#11674,#11675,#11676));
#3491=EDGE_LOOP('',(#11677,#11678,#11679,#11680,#11681));
#3492=EDGE_LOOP('',(#11682,#11683,#11684,#11685,#11686));
#3493=EDGE_LOOP('',(#11687,#11688,#11689,#11690,#11691,#11692));
#3494=EDGE_LOOP('',(#11693,#11694,#11695,#11696));
#3495=EDGE_LOOP('',(#11697,#11698,#11699,#11700,#11701));
#3496=EDGE_LOOP('',(#11702,#11703,#11704,#11705,#11706));
#3497=EDGE_LOOP('',(#11707,#11708,#11709,#11710,#11711,#11712));
#3498=EDGE_LOOP('',(#11713,#11714,#11715,#11716));
#3499=EDGE_LOOP('',(#11717,#11718,#11719,#11720,#11721));
#3500=EDGE_LOOP('',(#11722,#11723,#11724,#11725,#11726));
#3501=EDGE_LOOP('',(#11727,#11728,#11729,#11730,#11731,#11732));
#3502=EDGE_LOOP('',(#11733,#11734,#11735,#11736));
#3503=EDGE_LOOP('',(#11737,#11738,#11739,#11740,#11741));
#3504=EDGE_LOOP('',(#11742,#11743,#11744,#11745,#11746));
#3505=EDGE_LOOP('',(#11747,#11748,#11749,#11750,#11751,#11752));
#3506=EDGE_LOOP('',(#11753,#11754,#11755,#11756));
#3507=EDGE_LOOP('',(#11757,#11758,#11759,#11760));
#3508=EDGE_LOOP('',(#11761,#11762,#11763,#11764,#11765,#11766));
#3509=EDGE_LOOP('',(#11767,#11768,#11769,#11770,#11771,#11772));
#3510=EDGE_LOOP('',(#11773,#11774,#11775,#11776,#11777,#11778));
#3511=EDGE_LOOP('',(#11779,#11780,#11781,#11782));
#3512=EDGE_LOOP('',(#11783,#11784,#11785,#11786));
#3513=EDGE_LOOP('',(#11787,#11788,#11789,#11790));
#3514=EDGE_LOOP('',(#11791,#11792,#11793,#11794));
#3515=EDGE_LOOP('',(#11795,#11796,#11797,#11798));
#3516=EDGE_LOOP('',(#11799,#11800,#11801,#11802,#11803,#11804));
#3517=EDGE_LOOP('',(#11805,#11806,#11807,#11808,#11809,#11810));
#3518=EDGE_LOOP('',(#11811,#11812,#11813,#11814,#11815,#11816));
#3519=EDGE_LOOP('',(#11817,#11818,#11819,#11820,#11821,#11822));
#3520=EDGE_LOOP('',(#11823,#11824,#11825,#11826,#11827,#11828));
#3521=EDGE_LOOP('',(#11829,#11830,#11831,#11832));
#3522=EDGE_LOOP('',(#11833,#11834,#11835,#11836));
#3523=EDGE_LOOP('',(#11837,#11838,#11839,#11840));
#3524=EDGE_LOOP('',(#11841,#11842,#11843,#11844));
#3525=EDGE_LOOP('',(#11845,#11846,#11847,#11848,#11849));
#3526=EDGE_LOOP('',(#11850,#11851,#11852,#11853,#11854,#11855));
#3527=EDGE_LOOP('',(#11856,#11857,#11858,#11859));
#3528=EDGE_LOOP('',(#11860,#11861,#11862,#11863,#11864));
#3529=EDGE_LOOP('',(#11865,#11866,#11867,#11868,#11869));
#3530=EDGE_LOOP('',(#11870,#11871,#11872,#11873,#11874,#11875));
#3531=EDGE_LOOP('',(#11876,#11877,#11878,#11879));
#3532=EDGE_LOOP('',(#11880,#11881,#11882,#11883,#11884));
#3533=EDGE_LOOP('',(#11885,#11886,#11887,#11888,#11889));
#3534=EDGE_LOOP('',(#11890,#11891,#11892,#11893,#11894,#11895));
#3535=EDGE_LOOP('',(#11896,#11897,#11898,#11899));
#3536=EDGE_LOOP('',(#11900,#11901,#11902,#11903,#11904));
#3537=EDGE_LOOP('',(#11905,#11906,#11907,#11908,#11909));
#3538=EDGE_LOOP('',(#11910,#11911,#11912,#11913,#11914,#11915));
#3539=EDGE_LOOP('',(#11916,#11917,#11918,#11919));
#3540=EDGE_LOOP('',(#11920,#11921,#11922,#11923,#11924));
#3541=EDGE_LOOP('',(#11925,#11926,#11927,#11928,#11929));
#3542=EDGE_LOOP('',(#11930,#11931,#11932,#11933,#11934,#11935));
#3543=EDGE_LOOP('',(#11936,#11937,#11938,#11939));
#3544=EDGE_LOOP('',(#11940,#11941,#11942,#11943));
#3545=EDGE_LOOP('',(#11944,#11945,#11946,#11947));
#3546=EDGE_LOOP('',(#11948,#11949,#11950,#11951,#11952,#11953));
#3547=EDGE_LOOP('',(#11954,#11955,#11956,#11957,#11958));
#3548=EDGE_LOOP('',(#11959,#11960,#11961,#11962));
#3549=EDGE_LOOP('',(#11963,#11964,#11965,#11966,#11967,#11968));
#3550=EDGE_LOOP('',(#11969,#11970,#11971,#11972));
#3551=EDGE_LOOP('',(#11973,#11974,#11975,#11976,#11977));
#3552=EDGE_LOOP('',(#11978,#11979,#11980,#11981,#11982));
#3553=EDGE_LOOP('',(#11983,#11984,#11985,#11986,#11987,#11988));
#3554=EDGE_LOOP('',(#11989,#11990,#11991,#11992));
#3555=EDGE_LOOP('',(#11993,#11994,#11995,#11996,#11997));
#3556=EDGE_LOOP('',(#11998,#11999,#12000,#12001,#12002));
#3557=EDGE_LOOP('',(#12003,#12004,#12005,#12006,#12007,#12008));
#3558=EDGE_LOOP('',(#12009,#12010,#12011,#12012));
#3559=EDGE_LOOP('',(#12013,#12014,#12015,#12016,#12017));
#3560=EDGE_LOOP('',(#12018,#12019,#12020,#12021,#12022));
#3561=EDGE_LOOP('',(#12023,#12024,#12025,#12026,#12027,#12028));
#3562=EDGE_LOOP('',(#12029,#12030,#12031,#12032));
#3563=EDGE_LOOP('',(#12033,#12034,#12035,#12036));
#3564=EDGE_LOOP('',(#12037,#12038,#12039,#12040,#12041,#12042));
#3565=EDGE_LOOP('',(#12043,#12044,#12045,#12046,#12047,#12048));
#3566=EDGE_LOOP('',(#12049,#12050,#12051,#12052,#12053,#12054));
#3567=EDGE_LOOP('',(#12055,#12056,#12057,#12058,#12059,#12060));
#3568=EDGE_LOOP('',(#12061,#12062,#12063,#12064,#12065,#12066));
#3569=EDGE_LOOP('',(#12067,#12068,#12069,#12070));
#3570=EDGE_LOOP('',(#12071,#12072,#12073,#12074));
#3571=EDGE_LOOP('',(#12075,#12076,#12077,#12078));
#3572=EDGE_LOOP('',(#12079,#12080,#12081,#12082));
#3573=EDGE_LOOP('',(#12083,#12084,#12085,#12086));
#3574=EDGE_LOOP('',(#12087,#12088,#12089,#12090));
#3575=EDGE_LOOP('',(#12091,#12092,#12093,#12094,#12095,#12096));
#3576=EDGE_LOOP('',(#12097,#12098,#12099,#12100,#12101,#12102));
#3577=EDGE_LOOP('',(#12103,#12104,#12105,#12106,#12107,#12108));
#3578=EDGE_LOOP('',(#12109,#12110,#12111,#12112,#12113,#12114));
#3579=EDGE_LOOP('',(#12115,#12116,#12117,#12118));
#3580=EDGE_LOOP('',(#12119,#12120,#12121,#12122));
#3581=EDGE_LOOP('',(#12123,#12124,#12125,#12126));
#3582=EDGE_LOOP('',(#12127,#12128,#12129,#12130,#12131));
#3583=EDGE_LOOP('',(#12132,#12133,#12134,#12135,#12136,#12137));
#3584=EDGE_LOOP('',(#12138,#12139,#12140,#12141));
#3585=EDGE_LOOP('',(#12142,#12143,#12144,#12145,#12146));
#3586=EDGE_LOOP('',(#12147,#12148,#12149,#12150,#12151,#12152));
#3587=EDGE_LOOP('',(#12153,#12154,#12155,#12156,#12157));
#3588=EDGE_LOOP('',(#12158,#12159,#12160,#12161,#12162,#12163));
#3589=EDGE_LOOP('',(#12164,#12165,#12166,#12167));
#3590=EDGE_LOOP('',(#12168,#12169,#12170,#12171,#12172));
#3591=EDGE_LOOP('',(#12173,#12174,#12175,#12176,#12177));
#3592=EDGE_LOOP('',(#12178,#12179,#12180,#12181,#12182,#12183));
#3593=EDGE_LOOP('',(#12184,#12185,#12186,#12187));
#3594=EDGE_LOOP('',(#12188,#12189,#12190,#12191,#12192));
#3595=EDGE_LOOP('',(#12193,#12194,#12195,#12196,#12197));
#3596=EDGE_LOOP('',(#12198,#12199,#12200,#12201,#12202,#12203));
#3597=EDGE_LOOP('',(#12204,#12205,#12206,#12207));
#3598=EDGE_LOOP('',(#12208,#12209,#12210,#12211,#12212));
#3599=EDGE_LOOP('',(#12213,#12214,#12215,#12216,#12217));
#3600=EDGE_LOOP('',(#12218,#12219,#12220,#12221,#12222,#12223));
#3601=EDGE_LOOP('',(#12224,#12225,#12226,#12227));
#3602=EDGE_LOOP('',(#12228,#12229,#12230,#12231,#12232));
#3603=EDGE_LOOP('',(#12233,#12234,#12235,#12236,#12237));
#3604=EDGE_LOOP('',(#12238,#12239,#12240,#12241,#12242,#12243));
#3605=EDGE_LOOP('',(#12244,#12245,#12246,#12247));
#3606=EDGE_LOOP('',(#12248,#12249,#12250,#12251));
#3607=EDGE_LOOP('',(#12252,#12253,#12254,#12255));
#3608=EDGE_LOOP('',(#12256,#12257,#12258,#12259,#12260,#12261));
#3609=EDGE_LOOP('',(#12262,#12263,#12264,#12265,#12266));
#3610=EDGE_LOOP('',(#12267,#12268,#12269,#12270));
#3611=EDGE_LOOP('',(#12271,#12272,#12273,#12274,#12275,#12276));
#3612=EDGE_LOOP('',(#12277,#12278,#12279,#12280));
#3613=EDGE_LOOP('',(#12281,#12282,#12283,#12284,#12285));
#3614=EDGE_LOOP('',(#12286,#12287,#12288,#12289,#12290));
#3615=EDGE_LOOP('',(#12291,#12292,#12293,#12294,#12295,#12296));
#3616=EDGE_LOOP('',(#12297,#12298,#12299,#12300));
#3617=EDGE_LOOP('',(#12301,#12302,#12303,#12304,#12305));
#3618=EDGE_LOOP('',(#12306,#12307,#12308,#12309,#12310));
#3619=EDGE_LOOP('',(#12311,#12312,#12313,#12314,#12315,#12316));
#3620=EDGE_LOOP('',(#12317,#12318,#12319,#12320));
#3621=EDGE_LOOP('',(#12321,#12322,#12323,#12324));
#3622=EDGE_LOOP('',(#12325,#12326,#12327,#12328,#12329,#12330));
#3623=EDGE_LOOP('',(#12331,#12332,#12333,#12334,#12335,#12336));
#3624=EDGE_LOOP('',(#12337,#12338,#12339,#12340,#12341,#12342));
#3625=EDGE_LOOP('',(#12343,#12344,#12345,#12346,#12347,#12348));
#3626=EDGE_LOOP('',(#12349,#12350,#12351,#12352,#12353,#12354));
#3627=EDGE_LOOP('',(#12355,#12356,#12357,#12358));
#3628=EDGE_LOOP('',(#12359,#12360,#12361,#12362));
#3629=EDGE_LOOP('',(#12363,#12364,#12365,#12366));
#3630=EDGE_LOOP('',(#12367,#12368,#12369,#12370));
#3631=EDGE_LOOP('',(#12371,#12372,#12373,#12374));
#3632=EDGE_LOOP('',(#12375,#12376,#12377,#12378));
#3633=EDGE_LOOP('',(#12379,#12380,#12381,#12382));
#3634=EDGE_LOOP('',(#12383,#12384,#12385,#12386,#12387,#12388));
#3635=EDGE_LOOP('',(#12389,#12390,#12391,#12392,#12393,#12394));
#3636=EDGE_LOOP('',(#12395,#12396,#12397,#12398,#12399,#12400));
#3637=EDGE_LOOP('',(#12401,#12402,#12403,#12404));
#3638=EDGE_LOOP('',(#12405,#12406,#12407,#12408));
#3639=EDGE_LOOP('',(#12409,#12410,#12411,#12412,#12413));
#3640=EDGE_LOOP('',(#12414,#12415,#12416,#12417,#12418,#12419));
#3641=EDGE_LOOP('',(#12420,#12421,#12422,#12423));
#3642=EDGE_LOOP('',(#12424,#12425,#12426,#12427,#12428));
#3643=EDGE_LOOP('',(#12429,#12430,#12431,#12432,#12433));
#3644=EDGE_LOOP('',(#12434,#12435,#12436,#12437,#12438,#12439));
#3645=EDGE_LOOP('',(#12440,#12441,#12442,#12443));
#3646=EDGE_LOOP('',(#12444,#12445,#12446,#12447,#12448));
#3647=EDGE_LOOP('',(#12449,#12450,#12451,#12452,#12453));
#3648=EDGE_LOOP('',(#12454,#12455,#12456,#12457,#12458,#12459));
#3649=EDGE_LOOP('',(#12460,#12461,#12462,#12463));
#3650=EDGE_LOOP('',(#12464,#12465,#12466,#12467,#12468));
#3651=EDGE_LOOP('',(#12469,#12470,#12471,#12472,#12473));
#3652=EDGE_LOOP('',(#12474,#12475,#12476,#12477,#12478,#12479));
#3653=EDGE_LOOP('',(#12480,#12481,#12482,#12483));
#3654=EDGE_LOOP('',(#12484,#12485,#12486,#12487,#12488));
#3655=EDGE_LOOP('',(#12489,#12490,#12491,#12492,#12493));
#3656=EDGE_LOOP('',(#12494,#12495,#12496,#12497,#12498,#12499));
#3657=EDGE_LOOP('',(#12500,#12501,#12502,#12503));
#3658=EDGE_LOOP('',(#12504,#12505,#12506,#12507,#12508));
#3659=EDGE_LOOP('',(#12509,#12510,#12511,#12512,#12513));
#3660=EDGE_LOOP('',(#12514,#12515,#12516,#12517,#12518,#12519));
#3661=EDGE_LOOP('',(#12520,#12521,#12522,#12523));
#3662=EDGE_LOOP('',(#12524,#12525,#12526,#12527,#12528));
#3663=EDGE_LOOP('',(#12529,#12530,#12531,#12532,#12533));
#3664=EDGE_LOOP('',(#12534,#12535,#12536,#12537,#12538,#12539));
#3665=EDGE_LOOP('',(#12540,#12541,#12542,#12543));
#3666=EDGE_LOOP('',(#12544,#12545,#12546,#12547));
#3667=EDGE_LOOP('',(#12548,#12549,#12550,#12551));
#3668=EDGE_LOOP('',(#12552,#12553,#12554,#12555,#12556,#12557));
#3669=EDGE_LOOP('',(#12558,#12559,#12560,#12561,#12562));
#3670=EDGE_LOOP('',(#12563,#12564,#12565,#12566));
#3671=EDGE_LOOP('',(#12567,#12568,#12569,#12570,#12571,#12572));
#3672=EDGE_LOOP('',(#12573,#12574,#12575,#12576));
#3673=EDGE_LOOP('',(#12577,#12578,#12579,#12580,#12581));
#3674=EDGE_LOOP('',(#12582,#12583,#12584,#12585,#12586));
#3675=EDGE_LOOP('',(#12587,#12588,#12589,#12590,#12591,#12592));
#3676=EDGE_LOOP('',(#12593,#12594,#12595,#12596));
#3677=EDGE_LOOP('',(#12597,#12598,#12599,#12600));
#3678=EDGE_LOOP('',(#12601,#12602,#12603,#12604,#12605,#12606));
#3679=EDGE_LOOP('',(#12607,#12608,#12609,#12610,#12611,#12612));
#3680=EDGE_LOOP('',(#12613,#12614,#12615,#12616,#12617,#12618));
#3681=EDGE_LOOP('',(#12619,#12620,#12621,#12622,#12623,#12624));
#3682=EDGE_LOOP('',(#12625,#12626,#12627,#12628,#12629,#12630));
#3683=EDGE_LOOP('',(#12631,#12632,#12633,#12634,#12635,#12636));
#3684=EDGE_LOOP('',(#12637,#12638,#12639,#12640,#12641,#12642));
#3685=EDGE_LOOP('',(#12643,#12644,#12645,#12646));
#3686=EDGE_LOOP('',(#12647,#12648,#12649,#12650));
#3687=EDGE_LOOP('',(#12651,#12652,#12653,#12654));
#3688=EDGE_LOOP('',(#12655,#12656,#12657,#12658));
#3689=EDGE_LOOP('',(#12659,#12660,#12661,#12662));
#3690=EDGE_LOOP('',(#12663,#12664,#12665,#12666));
#3691=EDGE_LOOP('',(#12667,#12668,#12669,#12670));
#3692=EDGE_LOOP('',(#12671,#12672,#12673,#12674));
#3693=EDGE_LOOP('',(#12675,#12676,#12677,#12678,#12679,#12680));
#3694=EDGE_LOOP('',(#12681,#12682,#12683,#12684,#12685,#12686));
#3695=EDGE_LOOP('',(#12687,#12688,#12689,#12690));
#3696=EDGE_LOOP('',(#12691,#12692,#12693,#12694,#12695));
#3697=EDGE_LOOP('',(#12696,#12697,#12698,#12699,#12700,#12701));
#3698=EDGE_LOOP('',(#12702,#12703,#12704,#12705));
#3699=EDGE_LOOP('',(#12706,#12707,#12708,#12709,#12710));
#3700=EDGE_LOOP('',(#12711,#12712,#12713,#12714,#12715));
#3701=EDGE_LOOP('',(#12716,#12717,#12718,#12719,#12720,#12721));
#3702=EDGE_LOOP('',(#12722,#12723,#12724,#12725));
#3703=EDGE_LOOP('',(#12726,#12727,#12728,#12729,#12730));
#3704=EDGE_LOOP('',(#12731,#12732,#12733,#12734,#12735));
#3705=EDGE_LOOP('',(#12736,#12737,#12738,#12739,#12740,#12741));
#3706=EDGE_LOOP('',(#12742,#12743,#12744,#12745));
#3707=EDGE_LOOP('',(#12746,#12747,#12748,#12749,#12750));
#3708=EDGE_LOOP('',(#12751,#12752,#12753,#12754,#12755));
#3709=EDGE_LOOP('',(#12756,#12757,#12758,#12759,#12760,#12761));
#3710=EDGE_LOOP('',(#12762,#12763,#12764,#12765));
#3711=EDGE_LOOP('',(#12766,#12767,#12768,#12769,#12770));
#3712=EDGE_LOOP('',(#12771,#12772,#12773,#12774,#12775));
#3713=EDGE_LOOP('',(#12776,#12777,#12778,#12779,#12780,#12781));
#3714=EDGE_LOOP('',(#12782,#12783,#12784,#12785));
#3715=EDGE_LOOP('',(#12786,#12787,#12788,#12789,#12790));
#3716=EDGE_LOOP('',(#12791,#12792,#12793,#12794,#12795));
#3717=EDGE_LOOP('',(#12796,#12797,#12798,#12799,#12800,#12801));
#3718=EDGE_LOOP('',(#12802,#12803,#12804,#12805));
#3719=EDGE_LOOP('',(#12806,#12807,#12808,#12809,#12810));
#3720=EDGE_LOOP('',(#12811,#12812,#12813,#12814,#12815));
#3721=EDGE_LOOP('',(#12816,#12817,#12818,#12819,#12820,#12821));
#3722=EDGE_LOOP('',(#12822,#12823,#12824,#12825));
#3723=EDGE_LOOP('',(#12826,#12827,#12828,#12829,#12830));
#3724=EDGE_LOOP('',(#12831,#12832,#12833,#12834,#12835));
#3725=EDGE_LOOP('',(#12836,#12837,#12838,#12839,#12840,#12841));
#3726=EDGE_LOOP('',(#12842,#12843,#12844,#12845));
#3727=EDGE_LOOP('',(#12846,#12847,#12848,#12849));
#3728=EDGE_LOOP('',(#12850,#12851,#12852,#12853));
#3729=EDGE_LOOP('',(#12854,#12855,#12856,#12857,#12858,#12859));
#3730=EDGE_LOOP('',(#12860,#12861,#12862,#12863,#12864));
#3731=EDGE_LOOP('',(#12865,#12866,#12867,#12868));
#3732=EDGE_LOOP('',(#12869,#12870,#12871,#12872,#12873,#12874));
#3733=EDGE_LOOP('',(#12875,#12876,#12877,#12878));
#3734=EDGE_LOOP('',(#12879,#12880,#12881,#12882));
#3735=EDGE_LOOP('',(#12883,#12884,#12885,#12886,#12887,#12888));
#3736=EDGE_LOOP('',(#12889,#12890,#12891,#12892,#12893,#12894));
#3737=EDGE_LOOP('',(#12895,#12896,#12897,#12898,#12899,#12900));
#3738=EDGE_LOOP('',(#12901,#12902,#12903,#12904,#12905,#12906));
#3739=EDGE_LOOP('',(#12907,#12908,#12909,#12910,#12911,#12912));
#3740=EDGE_LOOP('',(#12913,#12914,#12915,#12916,#12917,#12918));
#3741=EDGE_LOOP('',(#12919,#12920,#12921,#12922,#12923,#12924));
#3742=EDGE_LOOP('',(#12925,#12926,#12927,#12928,#12929,#12930));
#3743=EDGE_LOOP('',(#12931,#12932,#12933,#12934));
#3744=EDGE_LOOP('',(#12935,#12936,#12937,#12938));
#3745=EDGE_LOOP('',(#12939,#12940,#12941,#12942));
#3746=EDGE_LOOP('',(#12943,#12944,#12945,#12946));
#3747=EDGE_LOOP('',(#12947,#12948,#12949,#12950));
#3748=EDGE_LOOP('',(#12951,#12952,#12953,#12954));
#3749=EDGE_LOOP('',(#12955,#12956,#12957,#12958));
#3750=EDGE_LOOP('',(#12959,#12960,#12961,#12962));
#3751=EDGE_LOOP('',(#12963,#12964,#12965,#12966));
#3752=EDGE_LOOP('',(#12967,#12968,#12969,#12970,#12971,#12972));
#3753=EDGE_LOOP('',(#12973,#12974,#12975,#12976,#12977));
#3754=EDGE_LOOP('',(#12978,#12979,#12980,#12981,#12982,#12983));
#3755=EDGE_LOOP('',(#12984,#12985,#12986,#12987));
#3756=EDGE_LOOP('',(#12988,#12989,#12990,#12991,#12992));
#3757=EDGE_LOOP('',(#12993,#12994,#12995,#12996,#12997));
#3758=EDGE_LOOP('',(#12998,#12999,#13000,#13001,#13002,#13003));
#3759=EDGE_LOOP('',(#13004,#13005,#13006,#13007));
#3760=EDGE_LOOP('',(#13008,#13009,#13010,#13011,#13012));
#3761=EDGE_LOOP('',(#13013,#13014,#13015,#13016,#13017));
#3762=EDGE_LOOP('',(#13018,#13019,#13020,#13021,#13022,#13023));
#3763=EDGE_LOOP('',(#13024,#13025,#13026,#13027));
#3764=EDGE_LOOP('',(#13028,#13029,#13030,#13031,#13032));
#3765=EDGE_LOOP('',(#13033,#13034,#13035,#13036,#13037));
#3766=EDGE_LOOP('',(#13038,#13039,#13040,#13041,#13042,#13043));
#3767=EDGE_LOOP('',(#13044,#13045,#13046,#13047));
#3768=EDGE_LOOP('',(#13048,#13049,#13050,#13051,#13052));
#3769=EDGE_LOOP('',(#13053,#13054,#13055,#13056,#13057));
#3770=EDGE_LOOP('',(#13058,#13059,#13060,#13061,#13062,#13063));
#3771=EDGE_LOOP('',(#13064,#13065,#13066,#13067));
#3772=EDGE_LOOP('',(#13068,#13069,#13070,#13071,#13072));
#3773=EDGE_LOOP('',(#13073,#13074,#13075,#13076,#13077));
#3774=EDGE_LOOP('',(#13078,#13079,#13080,#13081,#13082,#13083));
#3775=EDGE_LOOP('',(#13084,#13085,#13086,#13087));
#3776=EDGE_LOOP('',(#13088,#13089,#13090,#13091,#13092));
#3777=EDGE_LOOP('',(#13093,#13094,#13095,#13096,#13097));
#3778=EDGE_LOOP('',(#13098,#13099,#13100,#13101,#13102,#13103));
#3779=EDGE_LOOP('',(#13104,#13105,#13106,#13107));
#3780=EDGE_LOOP('',(#13108,#13109,#13110,#13111,#13112));
#3781=EDGE_LOOP('',(#13113,#13114,#13115,#13116,#13117));
#3782=EDGE_LOOP('',(#13118,#13119,#13120,#13121,#13122,#13123));
#3783=EDGE_LOOP('',(#13124,#13125,#13126,#13127));
#3784=EDGE_LOOP('',(#13128,#13129,#13130,#13131,#13132));
#3785=EDGE_LOOP('',(#13133,#13134,#13135,#13136,#13137));
#3786=EDGE_LOOP('',(#13138,#13139,#13140,#13141,#13142,#13143));
#3787=EDGE_LOOP('',(#13144,#13145,#13146,#13147));
#3788=EDGE_LOOP('',(#13148,#13149,#13150,#13151,#13152));
#3789=EDGE_LOOP('',(#13153,#13154,#13155,#13156));
#3790=EDGE_LOOP('',(#13157,#13158,#13159,#13160,#13161,#13162));
#3791=EDGE_LOOP('',(#13163,#13164,#13165,#13166,#13167));
#3792=EDGE_LOOP('',(#13168,#13169,#13170,#13171,#13172,#13173));
#3793=EDGE_LOOP('',(#13174,#13175,#13176,#13177,#13178,#13179));
#3794=EDGE_LOOP('',(#13180,#13181,#13182,#13183,#13184,#13185));
#3795=EDGE_LOOP('',(#13186,#13187,#13188,#13189,#13190,#13191));
#3796=EDGE_LOOP('',(#13192,#13193,#13194,#13195,#13196,#13197));
#3797=EDGE_LOOP('',(#13198,#13199,#13200,#13201,#13202,#13203));
#3798=EDGE_LOOP('',(#13204,#13205,#13206,#13207,#13208,#13209));
#3799=EDGE_LOOP('',(#13210,#13211,#13212,#13213,#13214,#13215));
#3800=EDGE_LOOP('',(#13216,#13217,#13218,#13219));
#3801=EDGE_LOOP('',(#13220,#13221,#13222,#13223));
#3802=EDGE_LOOP('',(#13224,#13225,#13226,#13227));
#3803=EDGE_LOOP('',(#13228,#13229,#13230,#13231));
#3804=EDGE_LOOP('',(#13232,#13233,#13234,#13235));
#3805=EDGE_LOOP('',(#13236,#13237,#13238,#13239));
#3806=EDGE_LOOP('',(#13240,#13241,#13242,#13243));
#3807=EDGE_LOOP('',(#13244,#13245,#13246,#13247));
#3808=EDGE_LOOP('',(#13248,#13249,#13250,#13251));
#3809=EDGE_LOOP('',(#13252,#13253,#13254,#13255));
#3810=EDGE_LOOP('',(#13256,#13257,#13258,#13259));
#3811=EDGE_LOOP('',(#13260,#13261,#13262,#13263,#13264,#13265));
#3812=EDGE_LOOP('',(#13266,#13267,#13268,#13269,#13270,#13271));
#3813=EDGE_LOOP('',(#13272,#13273,#13274,#13275,#13276,#13277));
#3814=EDGE_LOOP('',(#13278,#13279,#13280,#13281,#13282,#13283));
#3815=EDGE_LOOP('',(#13284,#13285,#13286,#13287,#13288,#13289));
#3816=EDGE_LOOP('',(#13290,#13291,#13292,#13293,#13294,#13295));
#3817=EDGE_LOOP('',(#13296,#13297,#13298,#13299,#13300,#13301));
#3818=EDGE_LOOP('',(#13302,#13303,#13304,#13305,#13306,#13307));
#3819=EDGE_LOOP('',(#13308,#13309,#13310,#13311));
#3820=EDGE_LOOP('',(#13312,#13313,#13314,#13315));
#3821=EDGE_LOOP('',(#13316,#13317,#13318,#13319));
#3822=EDGE_LOOP('',(#13320,#13321,#13322,#13323));
#3823=EDGE_LOOP('',(#13324,#13325,#13326,#13327));
#3824=EDGE_LOOP('',(#13328,#13329,#13330,#13331));
#3825=EDGE_LOOP('',(#13332,#13333,#13334,#13335));
#3826=EDGE_LOOP('',(#13336,#13337,#13338,#13339));
#3827=EDGE_LOOP('',(#13340,#13341,#13342,#13343));
#3828=EDGE_LOOP('',(#13344,#13345,#13346,#13347));
#3829=EDGE_LOOP('',(#13348,#13349,#13350,#13351,#13352,#13353));
#3830=EDGE_LOOP('',(#13354,#13355,#13356,#13357));
#3831=EDGE_LOOP('',(#13358,#13359,#13360,#13361,#13362,#13363));
#3832=EDGE_LOOP('',(#13364,#13365,#13366,#13367));
#3833=EDGE_LOOP('',(#13368,#13369,#13370,#13371,#13372,#13373));
#3834=EDGE_LOOP('',(#13374,#13375,#13376,#13377));
#3835=EDGE_LOOP('',(#13378,#13379,#13380,#13381,#13382,#13383));
#3836=EDGE_LOOP('',(#13384,#13385,#13386,#13387));
#3837=EDGE_LOOP('',(#13388,#13389,#13390,#13391,#13392,#13393));
#3838=EDGE_LOOP('',(#13394,#13395,#13396,#13397));
#3839=EDGE_LOOP('',(#13398,#13399,#13400,#13401,#13402,#13403));
#3840=EDGE_LOOP('',(#13404,#13405,#13406,#13407));
#3841=EDGE_LOOP('',(#13408,#13409,#13410,#13411,#13412,#13413));
#3842=EDGE_LOOP('',(#13414,#13415,#13416,#13417));
#3843=EDGE_LOOP('',(#13418,#13419,#13420,#13421,#13422,#13423));
#3844=EDGE_LOOP('',(#13424,#13425,#13426,#13427));
#3845=EDGE_LOOP('',(#13428,#13429,#13430,#13431,#13432,#13433));
#3846=EDGE_LOOP('',(#13434,#13435,#13436,#13437));
#3847=EDGE_LOOP('',(#13438,#13439,#13440,#13441,#13442,#13443));
#3848=EDGE_LOOP('',(#13444,#13445,#13446,#13447));
#3849=EDGE_LOOP('',(#13448,#13449,#13450,#13451,#13452,#13453));
#3850=EDGE_LOOP('',(#13454,#13455,#13456,#13457));
#3851=EDGE_LOOP('',(#13458,#13459,#13460,#13461,#13462,#13463));
#3852=EDGE_LOOP('',(#13464,#13465,#13466,#13467));
#3853=EDGE_LOOP('',(#13468,#13469,#13470,#13471));
#3854=EDGE_LOOP('',(#13472));
#3855=EDGE_LOOP('',(#13473));
#3856=EDGE_LOOP('',(#13474,#13475,#13476,#13477,#13478,#13479,#13480,#13481,
#13482,#13483,#13484,#13485,#13486,#13487,#13488,#13489,#13490,#13491,#13492,
#13493,#13494,#13495,#13496,#13497,#13498,#13499,#13500,#13501,#13502,#13503,
#13504,#13505,#13506,#13507,#13508,#13509,#13510,#13511,#13512,#13513,#13514,
#13515,#13516,#13517,#13518,#13519,#13520,#13521,#13522,#13523,#13524,#13525,
#13526,#13527,#13528,#13529,#13530,#13531,#13532,#13533,#13534,#13535,#13536,
#13537,#13538,#13539,#13540,#13541,#13542,#13543,#13544,#13545,#13546,#13547,
#13548,#13549,#13550,#13551,#13552,#13553,#13554,#13555,#13556,#13557,#13558,
#13559,#13560,#13561,#13562,#13563,#13564,#13565,#13566,#13567,#13568,#13569,
#13570,#13571,#13572,#13573,#13574,#13575,#13576,#13577,#13578,#13579,#13580,
#13581,#13582,#13583,#13584,#13585,#13586,#13587,#13588,#13589,#13590,#13591,
#13592,#13593,#13594,#13595,#13596,#13597,#13598,#13599,#13600,#13601,#13602,
#13603,#13604,#13605,#13606,#13607,#13608,#13609,#13610,#13611,#13612,#13613,
#13614,#13615,#13616,#13617,#13618,#13619,#13620,#13621,#13622,#13623,#13624,
#13625,#13626,#13627,#13628,#13629,#13630,#13631,#13632,#13633,#13634,#13635,
#13636,#13637,#13638,#13639,#13640,#13641,#13642,#13643,#13644,#13645,#13646,
#13647,#13648,#13649,#13650,#13651,#13652,#13653,#13654,#13655,#13656,#13657));
#3857=EDGE_LOOP('',(#13658,#13659,#13660,#13661));
#3858=EDGE_LOOP('',(#13662));
#3859=EDGE_LOOP('',(#13663));
#3860=EDGE_LOOP('',(#13664));
#3861=EDGE_LOOP('',(#13665));
#3862=EDGE_LOOP('',(#13666));
#3863=EDGE_LOOP('',(#13667));
#3864=EDGE_LOOP('',(#13668));
#3865=EDGE_LOOP('',(#13669,#13670,#13671,#13672));
#3866=EDGE_LOOP('',(#13673,#13674,#13675,#13676));
#3867=EDGE_LOOP('',(#13677,#13678,#13679,#13680));
#3868=EDGE_LOOP('',(#13681,#13682,#13683,#13684));
#3869=EDGE_LOOP('',(#13685,#13686,#13687,#13688));
#3870=EDGE_LOOP('',(#13689,#13690,#13691,#13692));
#3871=EDGE_LOOP('',(#13693,#13694,#13695,#13696));
#3872=EDGE_LOOP('',(#13697,#13698,#13699,#13700));
#3873=EDGE_LOOP('',(#13701,#13702,#13703,#13704));
#3874=EDGE_LOOP('',(#13705,#13706,#13707,#13708));
#3875=EDGE_LOOP('',(#13709,#13710,#13711,#13712));
#3876=EDGE_LOOP('',(#13713,#13714,#13715,#13716));
#3877=EDGE_LOOP('',(#13717,#13718,#13719,#13720));
#3878=EDGE_LOOP('',(#13721,#13722,#13723,#13724));
#3879=EDGE_LOOP('',(#13725,#13726,#13727,#13728));
#3880=EDGE_LOOP('',(#13729,#13730,#13731,#13732));
#3881=EDGE_LOOP('',(#13733,#13734,#13735,#13736));
#3882=EDGE_LOOP('',(#13737,#13738,#13739,#13740));
#3883=EDGE_LOOP('',(#13741,#13742,#13743,#13744));
#3884=EDGE_LOOP('',(#13745,#13746,#13747,#13748));
#3885=EDGE_LOOP('',(#13749,#13750,#13751,#13752));
#3886=EDGE_LOOP('',(#13753,#13754,#13755,#13756));
#3887=EDGE_LOOP('',(#13757,#13758,#13759,#13760));
#3888=EDGE_LOOP('',(#13761,#13762,#13763,#13764));
#3889=EDGE_LOOP('',(#13765,#13766,#13767,#13768));
#3890=EDGE_LOOP('',(#13769,#13770,#13771,#13772));
#3891=EDGE_LOOP('',(#13773,#13774,#13775,#13776));
#3892=EDGE_LOOP('',(#13777,#13778,#13779,#13780,#13781,#13782));
#3893=EDGE_LOOP('',(#13783,#13784,#13785,#13786));
#3894=EDGE_LOOP('',(#13787,#13788,#13789,#13790));
#3895=EDGE_LOOP('',(#13791,#13792,#13793,#13794));
#3896=EDGE_LOOP('',(#13795,#13796,#13797,#13798));
#3897=EDGE_LOOP('',(#13799,#13800,#13801,#13802));
#3898=EDGE_LOOP('',(#13803,#13804,#13805,#13806));
#3899=EDGE_LOOP('',(#13807,#13808,#13809,#13810));
#3900=EDGE_LOOP('',(#13811,#13812,#13813,#13814));
#3901=EDGE_LOOP('',(#13815,#13816,#13817,#13818));
#3902=EDGE_LOOP('',(#13819,#13820,#13821,#13822));
#3903=EDGE_LOOP('',(#13823,#13824,#13825,#13826,#13827,#13828));
#3904=EDGE_LOOP('',(#13829,#13830,#13831,#13832));
#3905=EDGE_LOOP('',(#13833,#13834,#13835,#13836));
#3906=EDGE_LOOP('',(#13837,#13838,#13839,#13840));
#3907=EDGE_LOOP('',(#13841,#13842,#13843,#13844));
#3908=EDGE_LOOP('',(#13845,#13846,#13847,#13848));
#3909=EDGE_LOOP('',(#13849,#13850,#13851,#13852));
#3910=EDGE_LOOP('',(#13853,#13854,#13855,#13856));
#3911=EDGE_LOOP('',(#13857,#13858,#13859,#13860));
#3912=EDGE_LOOP('',(#13861,#13862,#13863,#13864));
#3913=EDGE_LOOP('',(#13865,#13866,#13867,#13868));
#3914=EDGE_LOOP('',(#13869,#13870,#13871,#13872,#13873,#13874));
#3915=EDGE_LOOP('',(#13875,#13876,#13877,#13878));
#3916=EDGE_LOOP('',(#13879,#13880,#13881,#13882));
#3917=EDGE_LOOP('',(#13883,#13884,#13885,#13886));
#3918=EDGE_LOOP('',(#13887,#13888,#13889,#13890));
#3919=EDGE_LOOP('',(#13891,#13892,#13893,#13894));
#3920=EDGE_LOOP('',(#13895,#13896,#13897,#13898));
#3921=EDGE_LOOP('',(#13899,#13900,#13901,#13902));
#3922=EDGE_LOOP('',(#13903,#13904,#13905,#13906));
#3923=EDGE_LOOP('',(#13907,#13908,#13909,#13910));
#3924=EDGE_LOOP('',(#13911,#13912,#13913,#13914));
#3925=EDGE_LOOP('',(#13915,#13916,#13917,#13918));
#3926=EDGE_LOOP('',(#13919,#13920,#13921,#13922));
#3927=EDGE_LOOP('',(#13923,#13924,#13925,#13926));
#3928=EDGE_LOOP('',(#13927,#13928,#13929,#13930));
#3929=EDGE_LOOP('',(#13931,#13932,#13933,#13934));
#3930=EDGE_LOOP('',(#13935,#13936,#13937,#13938));
#3931=EDGE_LOOP('',(#13939,#13940,#13941,#13942));
#3932=EDGE_LOOP('',(#13943,#13944,#13945,#13946));
#3933=EDGE_LOOP('',(#13947,#13948,#13949,#13950,#13951));
#3934=EDGE_LOOP('',(#13952,#13953,#13954,#13955));
#3935=EDGE_LOOP('',(#13956,#13957,#13958,#13959));
#3936=EDGE_LOOP('',(#13960,#13961,#13962,#13963));
#3937=EDGE_LOOP('',(#13964,#13965,#13966,#13967));
#3938=EDGE_LOOP('',(#13968,#13969,#13970,#13971));
#3939=EDGE_LOOP('',(#13972,#13973,#13974,#13975));
#3940=EDGE_LOOP('',(#13976,#13977,#13978,#13979));
#3941=EDGE_LOOP('',(#13980,#13981,#13982,#13983));
#3942=EDGE_LOOP('',(#13984,#13985,#13986,#13987));
#3943=EDGE_LOOP('',(#13988,#13989,#13990,#13991));
#3944=EDGE_LOOP('',(#13992,#13993,#13994,#13995));
#3945=EDGE_LOOP('',(#13996,#13997,#13998,#13999));
#3946=EDGE_LOOP('',(#14000,#14001,#14002,#14003));
#3947=EDGE_LOOP('',(#14004,#14005,#14006,#14007));
#3948=EDGE_LOOP('',(#14008,#14009,#14010,#14011));
#3949=EDGE_LOOP('',(#14012,#14013,#14014,#14015));
#3950=EDGE_LOOP('',(#14016,#14017,#14018,#14019));
#3951=EDGE_LOOP('',(#14020,#14021,#14022,#14023));
#3952=EDGE_LOOP('',(#14024,#14025,#14026,#14027));
#3953=EDGE_LOOP('',(#14028,#14029,#14030,#14031));
#3954=EDGE_LOOP('',(#14032,#14033,#14034,#14035));
#3955=EDGE_LOOP('',(#14036,#14037,#14038,#14039));
#3956=EDGE_LOOP('',(#14040,#14041,#14042,#14043,#14044,#14045));
#3957=EDGE_LOOP('',(#14046,#14047,#14048,#14049));
#3958=EDGE_LOOP('',(#14050,#14051,#14052,#14053));
#3959=EDGE_LOOP('',(#14054,#14055,#14056,#14057));
#3960=EDGE_LOOP('',(#14058,#14059,#14060,#14061));
#3961=EDGE_LOOP('',(#14062,#14063,#14064,#14065));
#3962=EDGE_LOOP('',(#14066,#14067,#14068,#14069));
#3963=EDGE_LOOP('',(#14070,#14071,#14072,#14073));
#3964=EDGE_LOOP('',(#14074,#14075,#14076,#14077));
#3965=EDGE_LOOP('',(#14078,#14079,#14080,#14081));
#3966=EDGE_LOOP('',(#14082,#14083,#14084,#14085,#14086,#14087));
#3967=EDGE_LOOP('',(#14088,#14089,#14090,#14091));
#3968=EDGE_LOOP('',(#14092,#14093,#14094,#14095));
#3969=EDGE_LOOP('',(#14096,#14097,#14098,#14099));
#3970=EDGE_LOOP('',(#14100,#14101,#14102,#14103));
#3971=EDGE_LOOP('',(#14104,#14105,#14106,#14107));
#3972=EDGE_LOOP('',(#14108,#14109,#14110,#14111));
#3973=EDGE_LOOP('',(#14112,#14113,#14114,#14115));
#3974=EDGE_LOOP('',(#14116,#14117,#14118,#14119));
#3975=EDGE_LOOP('',(#14120,#14121,#14122,#14123));
#3976=EDGE_LOOP('',(#14124,#14125,#14126,#14127));
#3977=EDGE_LOOP('',(#14128,#14129,#14130,#14131,#14132,#14133));
#3978=EDGE_LOOP('',(#14134,#14135,#14136,#14137));
#3979=EDGE_LOOP('',(#14138,#14139,#14140,#14141));
#3980=EDGE_LOOP('',(#14142,#14143,#14144,#14145));
#3981=EDGE_LOOP('',(#14146,#14147,#14148,#14149));
#3982=EDGE_LOOP('',(#14150,#14151,#14152));
#3983=EDGE_LOOP('',(#14153,#14154,#14155));
#3984=EDGE_LOOP('',(#14156,#14157,#14158));
#3985=EDGE_LOOP('',(#14159,#14160,#14161));
#3986=EDGE_LOOP('',(#14162,#14163,#14164));
#3987=EDGE_LOOP('',(#14165,#14166,#14167,#14168));
#3988=EDGE_LOOP('',(#14169));
#3989=EDGE_LOOP('',(#14170));
#3990=EDGE_LOOP('',(#14171));
#3991=EDGE_LOOP('',(#14172));
#3992=EDGE_LOOP('',(#14173));
#3993=EDGE_LOOP('',(#14174));
#3994=EDGE_LOOP('',(#14175));
#3995=EDGE_LOOP('',(#14176));
#3996=EDGE_LOOP('',(#14177));
#3997=EDGE_LOOP('',(#14178));
#3998=EDGE_LOOP('',(#14179));
#3999=EDGE_LOOP('',(#14180));
#4000=EDGE_LOOP('',(#14181,#14182,#14183,#14184));
#4001=EDGE_LOOP('',(#14185,#14186,#14187,#14188));
#4002=EDGE_LOOP('',(#14189,#14190,#14191,#14192));
#4003=EDGE_LOOP('',(#14193,#14194,#14195,#14196));
#4004=EDGE_LOOP('',(#14197,#14198,#14199,#14200));
#4005=EDGE_LOOP('',(#14201,#14202,#14203,#14204));
#4006=EDGE_LOOP('',(#14205,#14206,#14207,#14208));
#4007=EDGE_LOOP('',(#14209,#14210,#14211,#14212));
#4008=EDGE_LOOP('',(#14213,#14214,#14215,#14216));
#4009=EDGE_LOOP('',(#14217,#14218,#14219,#14220));
#4010=EDGE_LOOP('',(#14221,#14222,#14223,#14224));
#4011=EDGE_LOOP('',(#14225,#14226,#14227,#14228));
#4012=EDGE_LOOP('',(#14229,#14230,#14231,#14232));
#4013=EDGE_LOOP('',(#14233,#14234,#14235,#14236));
#4014=EDGE_LOOP('',(#14237,#14238,#14239,#14240));
#4015=EDGE_LOOP('',(#14241,#14242,#14243,#14244));
#4016=EDGE_LOOP('',(#14245,#14246,#14247,#14248));
#4017=EDGE_LOOP('',(#14249,#14250,#14251,#14252));
#4018=EDGE_LOOP('',(#14253,#14254,#14255,#14256));
#4019=EDGE_LOOP('',(#14257,#14258,#14259,#14260));
#4020=EDGE_LOOP('',(#14261,#14262,#14263,#14264));
#4021=EDGE_LOOP('',(#14265,#14266,#14267,#14268));
#4022=EDGE_LOOP('',(#14269,#14270,#14271,#14272));
#4023=EDGE_LOOP('',(#14273,#14274,#14275,#14276));
#4024=EDGE_LOOP('',(#14277,#14278,#14279,#14280));
#4025=EDGE_LOOP('',(#14281,#14282,#14283,#14284,#14285,#14286,#14287,#14288,
#14289,#14290,#14291,#14292,#14293,#14294,#14295,#14296,#14297,#14298,#14299,
#14300,#14301,#14302,#14303,#14304,#14305,#14306,#14307,#14308));
#4026=EDGE_LOOP('',(#14309,#14310,#14311,#14312,#14313,#14314,#14315,#14316,
#14317,#14318,#14319,#14320,#14321,#14322,#14323,#14324,#14325,#14326,#14327,
#14328,#14329,#14330,#14331,#14332,#14333,#14334,#14335,#14336));
#4027=EDGE_LOOP('',(#14337));
#4028=EDGE_LOOP('',(#14338,#14339,#14340,#14341));
#4029=EDGE_LOOP('',(#14342,#14343,#14344,#14345));
#4030=EDGE_LOOP('',(#14346,#14347,#14348,#14349));
#4031=EDGE_LOOP('',(#14350));
#4032=EDGE_LOOP('',(#14351));
#4033=EDGE_LOOP('',(#14352,#14353,#14354,#14355));
#4034=EDGE_LOOP('',(#14356,#14357,#14358,#14359));
#4035=EDGE_LOOP('',(#14360));
#4036=EDGE_LOOP('',(#14361,#14362,#14363,#14364));
#4037=EDGE_LOOP('',(#14365,#14366,#14367,#14368));
#4038=EDGE_LOOP('',(#14369,#14370,#14371,#14372));
#4039=EDGE_LOOP('',(#14373,#14374,#14375,#14376));
#4040=EDGE_LOOP('',(#14377,#14378,#14379,#14380));
#4041=EDGE_LOOP('',(#14381,#14382,#14383,#14384));
#4042=EDGE_LOOP('',(#14385,#14386,#14387,#14388));
#4043=EDGE_LOOP('',(#14389,#14390,#14391,#14392));
#4044=EDGE_LOOP('',(#14393,#14394,#14395,#14396));
#4045=EDGE_LOOP('',(#14397,#14398,#14399,#14400));
#4046=EDGE_LOOP('',(#14401,#14402,#14403,#14404));
#4047=EDGE_LOOP('',(#14405,#14406,#14407,#14408));
#4048=EDGE_LOOP('',(#14409,#14410,#14411,#14412));
#4049=EDGE_LOOP('',(#14413,#14414,#14415,#14416,#14417));
#4050=EDGE_LOOP('',(#14418,#14419,#14420,#14421,#14422,#14423,#14424,#14425,
#14426,#14427,#14428,#14429,#14430,#14431,#14432,#14433));
#4051=EDGE_LOOP('',(#14434,#14435,#14436,#14437));
#4052=EDGE_LOOP('',(#14438,#14439,#14440,#14441,#14442,#14443,#14444,#14445,
#14446,#14447,#14448,#14449,#14450,#14451,#14452,#14453));
#4053=EDGE_LOOP('',(#14454,#14455,#14456,#14457));
#4054=EDGE_LOOP('',(#14458));
#4055=EDGE_LOOP('',(#14459,#14460,#14461,#14462));
#4056=EDGE_LOOP('',(#14463,#14464,#14465,#14466));
#4057=EDGE_LOOP('',(#14467));
#4058=EDGE_LOOP('',(#14468,#14469,#14470,#14471));
#4059=EDGE_LOOP('',(#14472,#14473,#14474,#14475,#14476,#14477));
#4060=EDGE_LOOP('',(#14478));
#4061=EDGE_LOOP('',(#14479,#14480,#14481,#14482,#14483,#14484));
#4062=EDGE_LOOP('',(#14485,#14486,#14487,#14488,#14489));
#4063=EDGE_LOOP('',(#14490,#14491,#14492,#14493,#14494));
#4064=EDGE_LOOP('',(#14495));
#4065=EDGE_LOOP('',(#14496));
#4066=EDGE_LOOP('',(#14497,#14498,#14499,#14500));
#4067=EDGE_LOOP('',(#14501,#14502,#14503,#14504));
#4068=EDGE_LOOP('',(#14505));
#4069=EDGE_LOOP('',(#14506,#14507,#14508,#14509));
#4070=EDGE_LOOP('',(#14510));
#4071=EDGE_LOOP('',(#14511));
#4072=EDGE_LOOP('',(#14512,#14513,#14514,#14515));
#4073=EDGE_LOOP('',(#14516));
#4074=EDGE_LOOP('',(#14517));
#4075=EDGE_LOOP('',(#14518));
#4076=EDGE_LOOP('',(#14519,#14520,#14521,#14522));
#4077=EDGE_LOOP('',(#14523));
#4078=EDGE_LOOP('',(#14524));
#4079=EDGE_LOOP('',(#14525,#14526,#14527,#14528));
#4080=EDGE_LOOP('',(#14529));
#4081=EDGE_LOOP('',(#14530));
#4082=EDGE_LOOP('',(#14531,#14532,#14533,#14534,#14535));
#4083=EDGE_LOOP('',(#14536,#14537,#14538,#14539,#14540));
#4084=EDGE_LOOP('',(#14541));
#4085=EDGE_LOOP('',(#14542));
#4086=EDGE_LOOP('',(#14543,#14544,#14545,#14546));
#4087=EDGE_LOOP('',(#14547));
#4088=EDGE_LOOP('',(#14548));
#4089=EDGE_LOOP('',(#14549,#14550,#14551,#14552));
#4090=EDGE_LOOP('',(#14553,#14554,#14555,#14556));
#4091=EDGE_LOOP('',(#14557,#14558,#14559,#14560));
#4092=EDGE_LOOP('',(#14561));
#4093=EDGE_LOOP('',(#14562));
#4094=EDGE_LOOP('',(#14563,#14564,#14565,#14566));
#4095=EDGE_LOOP('',(#14567));
#4096=EDGE_LOOP('',(#14568));
#4097=EDGE_LOOP('',(#14569,#14570,#14571,#14572,#14573,#14574,#14575,#14576,
#14577,#14578,#14579,#14580,#14581,#14582,#14583,#14584));
#4098=EDGE_LOOP('',(#14585,#14586,#14587,#14588,#14589,#14590));
#4099=EDGE_LOOP('',(#14591,#14592,#14593,#14594,#14595,#14596));
#4100=EDGE_LOOP('',(#14597,#14598,#14599));
#4101=EDGE_LOOP('',(#14600,#14601,#14602));
#4102=EDGE_LOOP('',(#14603,#14604,#14605));
#4103=EDGE_LOOP('',(#14606,#14607,#14608));
#4104=EDGE_LOOP('',(#14609,#14610,#14611));
#4105=EDGE_LOOP('',(#14612,#14613,#14614));
#4106=EDGE_LOOP('',(#14615,#14616,#14617,#14618,#14619,#14620));
#4107=EDGE_LOOP('',(#14621,#14622,#14623));
#4108=EDGE_LOOP('',(#14624,#14625,#14626));
#4109=EDGE_LOOP('',(#14627,#14628,#14629));
#4110=EDGE_LOOP('',(#14630,#14631,#14632));
#4111=EDGE_LOOP('',(#14633,#14634,#14635));
#4112=EDGE_LOOP('',(#14636,#14637,#14638));
#4113=EDGE_LOOP('',(#14639,#14640,#14641,#14642,#14643,#14644));
#4114=EDGE_LOOP('',(#14645,#14646,#14647,#14648));
#4115=EDGE_LOOP('',(#14649,#14650,#14651,#14652,#14653,#14654,#14655));
#4116=EDGE_LOOP('',(#14656,#14657,#14658,#14659));
#4117=EDGE_LOOP('',(#14660,#14661,#14662,#14663));
#4118=EDGE_LOOP('',(#14664,#14665,#14666,#14667,#14668,#14669));
#4119=EDGE_LOOP('',(#14670,#14671,#14672,#14673));
#4120=EDGE_LOOP('',(#14674,#14675,#14676,#14677));
#4121=EDGE_LOOP('',(#14678,#14679,#14680,#14681));
#4122=EDGE_LOOP('',(#14682,#14683,#14684,#14685));
#4123=EDGE_LOOP('',(#14686,#14687,#14688,#14689));
#4124=EDGE_LOOP('',(#14690,#14691,#14692,#14693));
#4125=EDGE_LOOP('',(#14694,#14695,#14696,#14697,#14698,#14699,#14700,#14701,
#14702,#14703,#14704,#14705,#14706,#14707,#14708,#14709));
#4126=EDGE_LOOP('',(#14710,#14711,#14712,#14713));
#4127=EDGE_LOOP('',(#14714,#14715,#14716,#14717,#14718));
#4128=EDGE_LOOP('',(#14719,#14720,#14721,#14722));
#4129=EDGE_LOOP('',(#14723,#14724));
#4130=EDGE_LOOP('',(#14725,#14726,#14727,#14728));
#4131=EDGE_LOOP('',(#14729));
#4132=EDGE_LOOP('',(#14730));
#4133=EDGE_LOOP('',(#14731,#14732,#14733,#14734));
#4134=EDGE_LOOP('',(#14735,#14736,#14737,#14738));
#4135=EDGE_LOOP('',(#14739,#14740,#14741,#14742));
#4136=EDGE_LOOP('',(#14743,#14744,#14745,#14746));
#4137=EDGE_LOOP('',(#14747,#14748,#14749,#14750));
#4138=EDGE_LOOP('',(#14751,#14752,#14753,#14754));
#4139=EDGE_LOOP('',(#14755,#14756,#14757,#14758));
#4140=EDGE_LOOP('',(#14759,#14760,#14761,#14762));
#4141=EDGE_LOOP('',(#14763,#14764,#14765,#14766,#14767));
#4142=EDGE_LOOP('',(#14768,#14769,#14770,#14771,#14772,#14773,#14774,#14775,
#14776,#14777,#14778,#14779));
#4143=EDGE_LOOP('',(#14780,#14781,#14782,#14783,#14784));
#4144=EDGE_LOOP('',(#14785,#14786,#14787,#14788));
#4145=EDGE_LOOP('',(#14789,#14790,#14791,#14792,#14793,#14794,#14795,#14796,
#14797,#14798,#14799,#14800));
#4146=EDGE_LOOP('',(#14801,#14802,#14803,#14804));
#4147=EDGE_LOOP('',(#14805,#14806,#14807,#14808));
#4148=EDGE_LOOP('',(#14809,#14810,#14811,#14812));
#4149=EDGE_LOOP('',(#14813,#14814,#14815,#14816));
#4150=EDGE_LOOP('',(#14817,#14818,#14819,#14820));
#4151=EDGE_LOOP('',(#14821,#14822,#14823,#14824));
#4152=EDGE_LOOP('',(#14825,#14826,#14827,#14828,#14829,#14830));
#4153=EDGE_LOOP('',(#14831));
#4154=EDGE_LOOP('',(#14832,#14833,#14834,#14835,#14836,#14837));
#4155=EDGE_LOOP('',(#14838,#14839,#14840,#14841));
#4156=EDGE_LOOP('',(#14842,#14843,#14844,#14845,#14846,#14847));
#4157=EDGE_LOOP('',(#14848));
#4158=EDGE_LOOP('',(#14849,#14850,#14851,#14852,#14853,#14854));
#4159=EDGE_LOOP('',(#14855,#14856,#14857,#14858));
#4160=EDGE_LOOP('',(#14859,#14860,#14861,#14862));
#4161=EDGE_LOOP('',(#14863,#14864,#14865,#14866));
#4162=EDGE_LOOP('',(#14867,#14868,#14869,#14870));
#4163=EDGE_LOOP('',(#14871,#14872,#14873,#14874));
#4164=EDGE_LOOP('',(#14875,#14876,#14877,#14878));
#4165=EDGE_LOOP('',(#14879,#14880,#14881,#14882));
#4166=EDGE_LOOP('',(#14883,#14884,#14885,#14886));
#4167=EDGE_LOOP('',(#14887,#14888,#14889,#14890));
#4168=EDGE_LOOP('',(#14891,#14892,#14893,#14894));
#4169=EDGE_LOOP('',(#14895,#14896,#14897,#14898));
#4170=EDGE_LOOP('',(#14899,#14900,#14901,#14902));
#4171=EDGE_LOOP('',(#14903,#14904,#14905,#14906));
#4172=EDGE_LOOP('',(#14907,#14908,#14909,#14910));
#4173=EDGE_LOOP('',(#14911,#14912,#14913,#14914));
#4174=EDGE_LOOP('',(#14915,#14916,#14917,#14918));
#4175=EDGE_LOOP('',(#14919,#14920,#14921,#14922));
#4176=EDGE_LOOP('',(#14923,#14924,#14925,#14926));
#4177=EDGE_LOOP('',(#14927,#14928,#14929,#14930));
#4178=EDGE_LOOP('',(#14931,#14932,#14933,#14934));
#4179=EDGE_LOOP('',(#14935,#14936,#14937,#14938));
#4180=EDGE_LOOP('',(#14939,#14940,#14941,#14942));
#4181=EDGE_LOOP('',(#14943,#14944,#14945,#14946));
#4182=EDGE_LOOP('',(#14947,#14948,#14949,#14950));
#4183=EDGE_LOOP('',(#14951,#14952,#14953,#14954));
#4184=EDGE_LOOP('',(#14955,#14956,#14957,#14958));
#4185=EDGE_LOOP('',(#14959,#14960,#14961,#14962));
#4186=EDGE_LOOP('',(#14963,#14964,#14965,#14966));
#4187=EDGE_LOOP('',(#14967,#14968,#14969,#14970));
#4188=EDGE_LOOP('',(#14971,#14972,#14973,#14974,#14975,#14976,#14977,#14978,
#14979,#14980,#14981,#14982,#14983,#14984,#14985,#14986,#14987,#14988,#14989,
#14990,#14991,#14992,#14993,#14994,#14995,#14996,#14997,#14998,#14999,#15000,
#15001,#15002,#15003));
#4189=EDGE_LOOP('',(#15004,#15005,#15006,#15007,#15008));
#4190=EDGE_LOOP('',(#15009,#15010,#15011,#15012));
#4191=EDGE_LOOP('',(#15013,#15014,#15015,#15016,#15017,#15018,#15019,#15020,
#15021,#15022,#15023,#15024,#15025,#15026,#15027,#15028,#15029,#15030,#15031,
#15032,#15033,#15034,#15035,#15036,#15037,#15038,#15039,#15040,#15041,#15042,
#15043,#15044,#15045));
#4192=EDGE_LOOP('',(#15046,#15047,#15048,#15049));
#4193=EDGE_LOOP('',(#15050,#15051,#15052));
#4194=EDGE_LOOP('',(#15053,#15054,#15055,#15056));
#4195=EDGE_LOOP('',(#15057,#15058,#15059,#15060,#15061,#15062,#15063,#15064,
#15065,#15066,#15067,#15068,#15069,#15070,#15071,#15072,#15073,#15074,#15075,
#15076,#15077,#15078,#15079,#15080,#15081,#15082,#15083,#15084,#15085,#15086,
#15087,#15088,#15089,#15090,#15091,#15092,#15093,#15094,#15095,#15096,#15097,
#15098,#15099,#15100,#15101,#15102,#15103,#15104,#15105,#15106,#15107,#15108,
#15109,#15110,#15111,#15112,#15113,#15114,#15115,#15116,#15117,#15118,#15119,
#15120,#15121,#15122,#15123,#15124,#15125,#15126,#15127,#15128,#15129,#15130,
#15131,#15132,#15133,#15134,#15135,#15136,#15137,#15138,#15139,#15140,#15141,
#15142,#15143,#15144,#15145,#15146,#15147,#15148,#15149,#15150,#15151,#15152,
#15153,#15154,#15155,#15156,#15157,#15158,#15159,#15160,#15161,#15162,#15163,
#15164,#15165,#15166,#15167,#15168,#15169,#15170,#15171,#15172,#15173,#15174,
#15175,#15176,#15177,#15178,#15179,#15180));
#4196=EDGE_LOOP('',(#15181,#15182,#15183,#15184));
#4197=EDGE_LOOP('',(#15185,#15186,#15187));
#4198=EDGE_LOOP('',(#15188,#15189,#15190,#15191));
#4199=EDGE_LOOP('',(#15192,#15193,#15194,#15195));
#4200=EDGE_LOOP('',(#15196,#15197,#15198));
#4201=EDGE_LOOP('',(#15199,#15200,#15201,#15202));
#4202=EDGE_LOOP('',(#15203,#15204,#15205,#15206));
#4203=EDGE_LOOP('',(#15207,#15208,#15209));
#4204=EDGE_LOOP('',(#15210,#15211,#15212,#15213));
#4205=EDGE_LOOP('',(#15214,#15215,#15216,#15217));
#4206=EDGE_LOOP('',(#15218,#15219,#15220));
#4207=EDGE_LOOP('',(#15221,#15222,#15223,#15224));
#4208=EDGE_LOOP('',(#15225,#15226,#15227,#15228));
#4209=EDGE_LOOP('',(#15229,#15230,#15231));
#4210=EDGE_LOOP('',(#15232,#15233,#15234,#15235));
#4211=EDGE_LOOP('',(#15236,#15237,#15238,#15239));
#4212=EDGE_LOOP('',(#15240,#15241,#15242));
#4213=EDGE_LOOP('',(#15243,#15244,#15245,#15246));
#4214=EDGE_LOOP('',(#15247,#15248,#15249,#15250));
#4215=EDGE_LOOP('',(#15251,#15252,#15253));
#4216=EDGE_LOOP('',(#15254,#15255,#15256,#15257));
#4217=EDGE_LOOP('',(#15258,#15259,#15260,#15261));
#4218=EDGE_LOOP('',(#15262,#15263,#15264));
#4219=EDGE_LOOP('',(#15265,#15266,#15267,#15268));
#4220=EDGE_LOOP('',(#15269,#15270,#15271,#15272));
#4221=EDGE_LOOP('',(#15273,#15274,#15275));
#4222=EDGE_LOOP('',(#15276,#15277,#15278,#15279));
#4223=EDGE_LOOP('',(#15280,#15281,#15282,#15283));
#4224=EDGE_LOOP('',(#15284,#15285,#15286));
#4225=EDGE_LOOP('',(#15287,#15288,#15289,#15290));
#4226=EDGE_LOOP('',(#15291,#15292,#15293,#15294));
#4227=EDGE_LOOP('',(#15295,#15296,#15297));
#4228=EDGE_LOOP('',(#15298,#15299,#15300,#15301));
#4229=EDGE_LOOP('',(#15302,#15303,#15304,#15305));
#4230=EDGE_LOOP('',(#15306,#15307,#15308));
#4231=EDGE_LOOP('',(#15309,#15310,#15311,#15312));
#4232=EDGE_LOOP('',(#15313,#15314,#15315,#15316));
#4233=EDGE_LOOP('',(#15317,#15318,#15319));
#4234=EDGE_LOOP('',(#15320,#15321,#15322,#15323));
#4235=EDGE_LOOP('',(#15324,#15325,#15326,#15327));
#4236=EDGE_LOOP('',(#15328,#15329,#15330,#15331));
#4237=EDGE_LOOP('',(#15332,#15333,#15334,#15335));
#4238=EDGE_LOOP('',(#15336,#15337,#15338,#15339));
#4239=EDGE_LOOP('',(#15340,#15341,#15342));
#4240=EDGE_LOOP('',(#15343,#15344,#15345,#15346));
#4241=EDGE_LOOP('',(#15347,#15348,#15349,#15350));
#4242=EDGE_LOOP('',(#15351,#15352,#15353));
#4243=EDGE_LOOP('',(#15354,#15355,#15356,#15357));
#4244=EDGE_LOOP('',(#15358,#15359,#15360,#15361));
#4245=EDGE_LOOP('',(#15362,#15363,#15364));
#4246=EDGE_LOOP('',(#15365,#15366,#15367,#15368));
#4247=EDGE_LOOP('',(#15369,#15370,#15371,#15372));
#4248=EDGE_LOOP('',(#15373,#15374,#15375));
#4249=EDGE_LOOP('',(#15376,#15377,#15378,#15379));
#4250=EDGE_LOOP('',(#15380,#15381,#15382,#15383));
#4251=EDGE_LOOP('',(#15384,#15385,#15386));
#4252=EDGE_LOOP('',(#15387,#15388,#15389,#15390));
#4253=EDGE_LOOP('',(#15391,#15392,#15393,#15394));
#4254=EDGE_LOOP('',(#15395,#15396,#15397));
#4255=EDGE_LOOP('',(#15398,#15399,#15400,#15401));
#4256=EDGE_LOOP('',(#15402,#15403,#15404,#15405));
#4257=EDGE_LOOP('',(#15406,#15407,#15408));
#4258=EDGE_LOOP('',(#15409,#15410,#15411,#15412));
#4259=EDGE_LOOP('',(#15413,#15414,#15415,#15416));
#4260=EDGE_LOOP('',(#15417,#15418,#15419));
#4261=EDGE_LOOP('',(#15420,#15421,#15422,#15423));
#4262=EDGE_LOOP('',(#15424,#15425,#15426,#15427));
#4263=EDGE_LOOP('',(#15428,#15429,#15430));
#4264=EDGE_LOOP('',(#15431,#15432,#15433,#15434));
#4265=EDGE_LOOP('',(#15435,#15436,#15437,#15438));
#4266=EDGE_LOOP('',(#15439,#15440,#15441));
#4267=EDGE_LOOP('',(#15442,#15443,#15444,#15445));
#4268=EDGE_LOOP('',(#15446,#15447,#15448,#15449));
#4269=EDGE_LOOP('',(#15450,#15451,#15452));
#4270=EDGE_LOOP('',(#15453,#15454,#15455,#15456));
#4271=EDGE_LOOP('',(#15457,#15458,#15459,#15460));
#4272=EDGE_LOOP('',(#15461,#15462,#15463));
#4273=EDGE_LOOP('',(#15464,#15465,#15466,#15467));
#4274=EDGE_LOOP('',(#15468,#15469,#15470,#15471));
#4275=EDGE_LOOP('',(#15472,#15473,#15474));
#4276=EDGE_LOOP('',(#15475,#15476,#15477,#15478));
#4277=EDGE_LOOP('',(#15479,#15480,#15481,#15482));
#4278=EDGE_LOOP('',(#15483,#15484,#15485));
#4279=EDGE_LOOP('',(#15486,#15487,#15488,#15489));
#4280=EDGE_LOOP('',(#15490,#15491,#15492,#15493));
#4281=EDGE_LOOP('',(#15494,#15495,#15496));
#4282=EDGE_LOOP('',(#15497,#15498,#15499,#15500));
#4283=EDGE_LOOP('',(#15501));
#4284=EDGE_LOOP('',(#15502,#15503,#15504,#15505,#15506,#15507));
#4285=EDGE_LOOP('',(#15508,#15509,#15510,#15511));
#4286=EDGE_LOOP('',(#15512));
#4287=EDGE_LOOP('',(#15513,#15514,#15515,#15516));
#4288=EDGE_LOOP('',(#15517,#15518,#15519,#15520));
#4289=EDGE_LOOP('',(#15521,#15522,#15523,#15524,#15525,#15526,#15527,#15528,
#15529,#15530,#15531,#15532,#15533,#15534,#15535,#15536,#15537,#15538,#15539,
#15540,#15541,#15542,#15543,#15544,#15545,#15546,#15547,#15548,#15549,#15550,
#15551,#15552,#15553,#15554,#15555,#15556,#15557,#15558,#15559,#15560,#15561,
#15562,#15563,#15564,#15565,#15566,#15567,#15568,#15569,#15570,#15571,#15572,
#15573,#15574,#15575,#15576,#15577,#15578,#15579,#15580,#15581,#15582,#15583,
#15584,#15585,#15586,#15587,#15588,#15589,#15590,#15591,#15592,#15593,#15594,
#15595,#15596,#15597,#15598,#15599,#15600,#15601,#15602,#15603,#15604,#15605,
#15606,#15607,#15608,#15609,#15610,#15611,#15612,#15613));
#4290=EDGE_LOOP('',(#15614));
#4291=LINE('',#23621,#5266);
#4292=LINE('',#23623,#5267);
#4293=LINE('',#23625,#5268);
#4294=LINE('',#23626,#5269);
#4295=LINE('',#23630,#5270);
#4296=LINE('',#23632,#5271);
#4297=LINE('',#23634,#5272);
#4298=LINE('',#23635,#5273);
#4299=LINE('',#23637,#5274);
#4300=LINE('',#23638,#5275);
#4301=LINE('',#23640,#5276);
#4302=LINE('',#23641,#5277);
#4303=LINE('',#23644,#5278);
#4304=LINE('',#23646,#5279);
#4305=LINE('',#23647,#5280);
#4306=LINE('',#23650,#5281);
#4307=LINE('',#23651,#5282);
#4308=LINE('',#23655,#5283);
#4309=LINE('',#23657,#5284);
#4310=LINE('',#23659,#5285);
#4311=LINE('',#23665,#5286);
#4312=LINE('',#23667,#5287);
#4313=LINE('',#23669,#5288);
#4314=LINE('',#23670,#5289);
#4315=LINE('',#23673,#5290);
#4316=LINE('',#23675,#5291);
#4317=LINE('',#23677,#5292);
#4318=LINE('',#23678,#5293);
#4319=LINE('',#23681,#5294);
#4320=LINE('',#23683,#5295);
#4321=LINE('',#23685,#5296);
#4322=LINE('',#23686,#5297);
#4323=LINE('',#23690,#5298);
#4324=LINE('',#23691,#5299);
#4325=LINE('',#23692,#5300);
#4326=LINE('',#23695,#5301);
#4327=LINE('',#23696,#5302);
#4328=LINE('',#23699,#5303);
#4329=LINE('',#23700,#5304);
#4330=LINE('',#23703,#5305);
#4331=LINE('',#23705,#5306);
#4332=LINE('',#23706,#5307);
#4333=LINE('',#23709,#5308);
#4334=LINE('',#23710,#5309);
#4335=LINE('',#23713,#5310);
#4336=LINE('',#23714,#5311);
#4337=LINE('',#23717,#5312);
#4338=LINE('',#23719,#5313);
#4339=LINE('',#23720,#5314);
#4340=LINE('',#23723,#5315);
#4341=LINE('',#23725,#5316);
#4342=LINE('',#23726,#5317);
#4343=LINE('',#23729,#5318);
#4344=LINE('',#23731,#5319);
#4345=LINE('',#23732,#5320);
#4346=LINE('',#23735,#5321);
#4347=LINE('',#23737,#5322);
#4348=LINE('',#23738,#5323);
#4349=LINE('',#23741,#5324);
#4350=LINE('',#23743,#5325);
#4351=LINE('',#23744,#5326);
#4352=LINE('',#23747,#5327);
#4353=LINE('',#23749,#5328);
#4354=LINE('',#23750,#5329);
#4355=LINE('',#23753,#5330);
#4356=LINE('',#23755,#5331);
#4357=LINE('',#23756,#5332);
#4358=LINE('',#23759,#5333);
#4359=LINE('',#23761,#5334);
#4360=LINE('',#23762,#5335);
#4361=LINE('',#23766,#5336);
#4362=LINE('',#23767,#5337);
#4363=LINE('',#23768,#5338);
#4364=LINE('',#23772,#5339);
#4365=LINE('',#23775,#5340);
#4366=LINE('',#23777,#5341);
#4367=LINE('',#23778,#5342);
#4368=LINE('',#23782,#5343);
#4369=LINE('',#23786,#5344);
#4370=LINE('',#23787,#5345);
#4371=LINE('',#23789,#5346);
#4372=LINE('',#23790,#5347);
#4373=LINE('',#23792,#5348);
#4374=LINE('',#23796,#5349);
#4375=LINE('',#23797,#5350);
#4376=LINE('',#23799,#5351);
#4377=LINE('',#23800,#5352);
#4378=LINE('',#23803,#5353);
#4379=LINE('',#23811,#5354);
#4380=LINE('',#23813,#5355);
#4381=LINE('',#23828,#5356);
#4382=LINE('',#23836,#5357);
#4383=LINE('',#23877,#5358);
#4384=LINE('',#23879,#5359);
#4385=LINE('',#23881,#5360);
#4386=LINE('',#23895,#5361);
#4387=LINE('',#23897,#5362);
#4388=LINE('',#23899,#5363);
#4389=LINE('',#23901,#5364);
#4390=LINE('',#23903,#5365);
#4391=LINE('',#23905,#5366);
#4392=LINE('',#23907,#5367);
#4393=LINE('',#23909,#5368);
#4394=LINE('',#23911,#5369);
#4395=LINE('',#23913,#5370);
#4396=LINE('',#23916,#5371);
#4397=LINE('',#23920,#5372);
#4398=LINE('',#23923,#5373);
#4399=LINE('',#23924,#5374);
#4400=LINE('',#23928,#5375);
#4401=LINE('',#23931,#5376);
#4402=LINE('',#23939,#5377);
#4403=LINE('',#23944,#5378);
#4404=LINE('',#23946,#5379);
#4405=LINE('',#23949,#5380);
#4406=LINE('',#23954,#5381);
#4407=LINE('',#23957,#5382);
#4408=LINE('',#23967,#5383);
#4409=LINE('',#23970,#5384);
#4410=LINE('',#23977,#5385);
#4411=LINE('',#23980,#5386);
#4412=LINE('',#23988,#5387);
#4413=LINE('',#23989,#5388);
#4414=LINE('',#23991,#5389);
#4415=LINE('',#24001,#5390);
#4416=LINE('',#24003,#5391);
#4417=LINE('',#24004,#5392);
#4418=LINE('',#24009,#5393);
#4419=LINE('',#24034,#5394);
#4420=LINE('',#24036,#5395);
#4421=LINE('',#24038,#5396);
#4422=LINE('',#24046,#5397);
#4423=LINE('',#24066,#5398);
#4424=LINE('',#24067,#5399);
#4425=LINE('',#24077,#5400);
#4426=LINE('',#24086,#5401);
#4427=LINE('',#24088,#5402);
#4428=LINE('',#24090,#5403);
#4429=LINE('',#24115,#5404);
#4430=LINE('',#24119,#5405);
#4431=LINE('',#24121,#5406);
#4432=LINE('',#24130,#5407);
#4433=LINE('',#24148,#5408);
#4434=LINE('',#24150,#5409);
#4435=LINE('',#24152,#5410);
#4436=LINE('',#24177,#5411);
#4437=LINE('',#24180,#5412);
#4438=LINE('',#24182,#5413);
#4439=LINE('',#24188,#5414);
#4440=LINE('',#24190,#5415);
#4441=LINE('',#24197,#5416);
#4442=LINE('',#24199,#5417);
#4443=LINE('',#24204,#5418);
#4444=LINE('',#24219,#5419);
#4445=LINE('',#24242,#5420);
#4446=LINE('',#24244,#5421);
#4447=LINE('',#24246,#5422);
#4448=LINE('',#24254,#5423);
#4449=LINE('',#24276,#5424);
#4450=LINE('',#24278,#5425);
#4451=LINE('',#24287,#5426);
#4452=LINE('',#24309,#5427);
#4453=LINE('',#24312,#5428);
#4454=LINE('',#24314,#5429);
#4455=LINE('',#24321,#5430);
#4456=LINE('',#24323,#5431);
#4457=LINE('',#24332,#5432);
#4458=LINE('',#24354,#5433);
#4459=LINE('',#24357,#5434);
#4460=LINE('',#24359,#5435);
#4461=LINE('',#24366,#5436);
#4462=LINE('',#24368,#5437);
#4463=LINE('',#24377,#5438);
#4464=LINE('',#24399,#5439);
#4465=LINE('',#24402,#5440);
#4466=LINE('',#24404,#5441);
#4467=LINE('',#24411,#5442);
#4468=LINE('',#24413,#5443);
#4469=LINE('',#24422,#5444);
#4470=LINE('',#24444,#5445);
#4471=LINE('',#24447,#5446);
#4472=LINE('',#24449,#5447);
#4473=LINE('',#24456,#5448);
#4474=LINE('',#24458,#5449);
#4475=LINE('',#24467,#5450);
#4476=LINE('',#24489,#5451);
#4477=LINE('',#24492,#5452);
#4478=LINE('',#24494,#5453);
#4479=LINE('',#24501,#5454);
#4480=LINE('',#24503,#5455);
#4481=LINE('',#24512,#5456);
#4482=LINE('',#24534,#5457);
#4483=LINE('',#24537,#5458);
#4484=LINE('',#24539,#5459);
#4485=LINE('',#24546,#5460);
#4486=LINE('',#24548,#5461);
#4487=LINE('',#24557,#5462);
#4488=LINE('',#24579,#5463);
#4489=LINE('',#24582,#5464);
#4490=LINE('',#24584,#5465);
#4491=LINE('',#24591,#5466);
#4492=LINE('',#24593,#5467);
#4493=LINE('',#24602,#5468);
#4494=LINE('',#24624,#5469);
#4495=LINE('',#24627,#5470);
#4496=LINE('',#24629,#5471);
#4497=LINE('',#24978,#5472);
#4498=LINE('',#24982,#5473);
#4499=LINE('',#24989,#5474);
#4500=LINE('',#24990,#5475);
#4501=LINE('',#24998,#5476);
#4502=LINE('',#25000,#5477);
#4503=LINE('',#25002,#5478);
#4504=LINE('',#25024,#5479);
#4505=LINE('',#25027,#5480);
#4506=LINE('',#25029,#5481);
#4507=LINE('',#25040,#5482);
#4508=LINE('',#25042,#5483);
#4509=LINE('',#25044,#5484);
#4510=LINE('',#25066,#5485);
#4511=LINE('',#25069,#5486);
#4512=LINE('',#25071,#5487);
#4513=LINE('',#25082,#5488);
#4514=LINE('',#25084,#5489);
#4515=LINE('',#25086,#5490);
#4516=LINE('',#25108,#5491);
#4517=LINE('',#25115,#5492);
#4518=LINE('',#25116,#5493);
#4519=LINE('',#25121,#5494);
#4520=LINE('',#25128,#5495);
#4521=LINE('',#25132,#5496);
#4522=LINE('',#25134,#5497);
#4523=LINE('',#25139,#5498);
#4524=LINE('',#25158,#5499);
#4525=LINE('',#25161,#5500);
#4526=LINE('',#25163,#5501);
#4527=LINE('',#25170,#5502);
#4528=LINE('',#25172,#5503);
#4529=LINE('',#25181,#5504);
#4530=LINE('',#25200,#5505);
#4531=LINE('',#25203,#5506);
#4532=LINE('',#25205,#5507);
#4533=LINE('',#25212,#5508);
#4534=LINE('',#25214,#5509);
#4535=LINE('',#25223,#5510);
#4536=LINE('',#25242,#5511);
#4537=LINE('',#25245,#5512);
#4538=LINE('',#25247,#5513);
#4539=LINE('',#25254,#5514);
#4540=LINE('',#25256,#5515);
#4541=LINE('',#25265,#5516);
#4542=LINE('',#25284,#5517);
#4543=LINE('',#25287,#5518);
#4544=LINE('',#25289,#5519);
#4545=LINE('',#25296,#5520);
#4546=LINE('',#25298,#5521);
#4547=LINE('',#25307,#5522);
#4548=LINE('',#25326,#5523);
#4549=LINE('',#25329,#5524);
#4550=LINE('',#25331,#5525);
#4551=LINE('',#25338,#5526);
#4552=LINE('',#25340,#5527);
#4553=LINE('',#25349,#5528);
#4554=LINE('',#25368,#5529);
#4555=LINE('',#25372,#5530);
#4556=LINE('',#25374,#5531);
#4557=LINE('',#25376,#5532);
#4558=LINE('',#25399,#5533);
#4559=LINE('',#25400,#5534);
#4560=LINE('',#25430,#5535);
#4561=LINE('',#25432,#5536);
#4562=LINE('',#25434,#5537);
#4563=LINE('',#25456,#5538);
#4564=LINE('',#25459,#5539);
#4565=LINE('',#25461,#5540);
#4566=LINE('',#25478,#5541);
#4567=LINE('',#25480,#5542);
#4568=LINE('',#25482,#5543);
#4569=LINE('',#25500,#5544);
#4570=LINE('',#25503,#5545);
#4571=LINE('',#25505,#5546);
#4572=LINE('',#25516,#5547);
#4573=LINE('',#25518,#5548);
#4574=LINE('',#25520,#5549);
#4575=LINE('',#25542,#5550);
#4576=LINE('',#25545,#5551);
#4577=LINE('',#25547,#5552);
#4578=LINE('',#25558,#5553);
#4579=LINE('',#25560,#5554);
#4580=LINE('',#25562,#5555);
#4581=LINE('',#25584,#5556);
#4582=LINE('',#25592,#5557);
#4583=LINE('',#25594,#5558);
#4584=LINE('',#25595,#5559);
#4585=LINE('',#25600,#5560);
#4586=LINE('',#25611,#5561);
#4587=LINE('',#25615,#5562);
#4588=LINE('',#25617,#5563);
#4589=LINE('',#25622,#5564);
#4590=LINE('',#25641,#5565);
#4591=LINE('',#25644,#5566);
#4592=LINE('',#25646,#5567);
#4593=LINE('',#25653,#5568);
#4594=LINE('',#25655,#5569);
#4595=LINE('',#25664,#5570);
#4596=LINE('',#25683,#5571);
#4597=LINE('',#25686,#5572);
#4598=LINE('',#25688,#5573);
#4599=LINE('',#25695,#5574);
#4600=LINE('',#25697,#5575);
#4601=LINE('',#25706,#5576);
#4602=LINE('',#25725,#5577);
#4603=LINE('',#25728,#5578);
#4604=LINE('',#25730,#5579);
#4605=LINE('',#25737,#5580);
#4606=LINE('',#25739,#5581);
#4607=LINE('',#25748,#5582);
#4608=LINE('',#25767,#5583);
#4609=LINE('',#25770,#5584);
#4610=LINE('',#25772,#5585);
#4611=LINE('',#25779,#5586);
#4612=LINE('',#25781,#5587);
#4613=LINE('',#25790,#5588);
#4614=LINE('',#25809,#5589);
#4615=LINE('',#25813,#5590);
#4616=LINE('',#25815,#5591);
#4617=LINE('',#25817,#5592);
#4618=LINE('',#25842,#5593);
#4619=LINE('',#25843,#5594);
#4620=LINE('',#25869,#5595);
#4621=LINE('',#25871,#5596);
#4622=LINE('',#25873,#5597);
#4623=LINE('',#25895,#5598);
#4624=LINE('',#25898,#5599);
#4625=LINE('',#25900,#5600);
#4626=LINE('',#25911,#5601);
#4627=LINE('',#25913,#5602);
#4628=LINE('',#25915,#5603);
#4629=LINE('',#25937,#5604);
#4630=LINE('',#25940,#5605);
#4631=LINE('',#25942,#5606);
#4632=LINE('',#25953,#5607);
#4633=LINE('',#25955,#5608);
#4634=LINE('',#25957,#5609);
#4635=LINE('',#25979,#5610);
#4636=LINE('',#25982,#5611);
#4637=LINE('',#25984,#5612);
#4638=LINE('',#25995,#5613);
#4639=LINE('',#25997,#5614);
#4640=LINE('',#25999,#5615);
#4641=LINE('',#26021,#5616);
#4642=LINE('',#26024,#5617);
#4643=LINE('',#26026,#5618);
#4644=LINE('',#26037,#5619);
#4645=LINE('',#26039,#5620);
#4646=LINE('',#26041,#5621);
#4647=LINE('',#26063,#5622);
#4648=LINE('',#26071,#5623);
#4649=LINE('',#26073,#5624);
#4650=LINE('',#26074,#5625);
#4651=LINE('',#26079,#5626);
#4652=LINE('',#26090,#5627);
#4653=LINE('',#26094,#5628);
#4654=LINE('',#26096,#5629);
#4655=LINE('',#26101,#5630);
#4656=LINE('',#26120,#5631);
#4657=LINE('',#26123,#5632);
#4658=LINE('',#26125,#5633);
#4659=LINE('',#26132,#5634);
#4660=LINE('',#26134,#5635);
#4661=LINE('',#26143,#5636);
#4662=LINE('',#26162,#5637);
#4663=LINE('',#26165,#5638);
#4664=LINE('',#26167,#5639);
#4665=LINE('',#26174,#5640);
#4666=LINE('',#26176,#5641);
#4667=LINE('',#26185,#5642);
#4668=LINE('',#26204,#5643);
#4669=LINE('',#26207,#5644);
#4670=LINE('',#26209,#5645);
#4671=LINE('',#26216,#5646);
#4672=LINE('',#26218,#5647);
#4673=LINE('',#26227,#5648);
#4674=LINE('',#26246,#5649);
#4675=LINE('',#26250,#5650);
#4676=LINE('',#26252,#5651);
#4677=LINE('',#26254,#5652);
#4678=LINE('',#26285,#5653);
#4679=LINE('',#26286,#5654);
#4680=LINE('',#26308,#5655);
#4681=LINE('',#26310,#5656);
#4682=LINE('',#26312,#5657);
#4683=LINE('',#26334,#5658);
#4684=LINE('',#26337,#5659);
#4685=LINE('',#26339,#5660);
#4686=LINE('',#26356,#5661);
#4687=LINE('',#26358,#5662);
#4688=LINE('',#26360,#5663);
#4689=LINE('',#26378,#5664);
#4690=LINE('',#26381,#5665);
#4691=LINE('',#26383,#5666);
#4692=LINE('',#26394,#5667);
#4693=LINE('',#26396,#5668);
#4694=LINE('',#26398,#5669);
#4695=LINE('',#26420,#5670);
#4696=LINE('',#26423,#5671);
#4697=LINE('',#26425,#5672);
#4698=LINE('',#26436,#5673);
#4699=LINE('',#26438,#5674);
#4700=LINE('',#26440,#5675);
#4701=LINE('',#26462,#5676);
#4702=LINE('',#26465,#5677);
#4703=LINE('',#26467,#5678);
#4704=LINE('',#26478,#5679);
#4705=LINE('',#26480,#5680);
#4706=LINE('',#26482,#5681);
#4707=LINE('',#26504,#5682);
#4708=LINE('',#26507,#5683);
#4709=LINE('',#26509,#5684);
#4710=LINE('',#26520,#5685);
#4711=LINE('',#26522,#5686);
#4712=LINE('',#26524,#5687);
#4713=LINE('',#26546,#5688);
#4714=LINE('',#26554,#5689);
#4715=LINE('',#26556,#5690);
#4716=LINE('',#26557,#5691);
#4717=LINE('',#26562,#5692);
#4718=LINE('',#26573,#5693);
#4719=LINE('',#26577,#5694);
#4720=LINE('',#26579,#5695);
#4721=LINE('',#26584,#5696);
#4722=LINE('',#26603,#5697);
#4723=LINE('',#26606,#5698);
#4724=LINE('',#26608,#5699);
#4725=LINE('',#26615,#5700);
#4726=LINE('',#26617,#5701);
#4727=LINE('',#26626,#5702);
#4728=LINE('',#26645,#5703);
#4729=LINE('',#26648,#5704);
#4730=LINE('',#26650,#5705);
#4731=LINE('',#26657,#5706);
#4732=LINE('',#26659,#5707);
#4733=LINE('',#26668,#5708);
#4734=LINE('',#26687,#5709);
#4735=LINE('',#26691,#5710);
#4736=LINE('',#26693,#5711);
#4737=LINE('',#26695,#5712);
#4738=LINE('',#26728,#5713);
#4739=LINE('',#26729,#5714);
#4740=LINE('',#26747,#5715);
#4741=LINE('',#26749,#5716);
#4742=LINE('',#26751,#5717);
#4743=LINE('',#26773,#5718);
#4744=LINE('',#26776,#5719);
#4745=LINE('',#26778,#5720);
#4746=LINE('',#26789,#5721);
#4747=LINE('',#26791,#5722);
#4748=LINE('',#26793,#5723);
#4749=LINE('',#26815,#5724);
#4750=LINE('',#26818,#5725);
#4751=LINE('',#26820,#5726);
#4752=LINE('',#26831,#5727);
#4753=LINE('',#26833,#5728);
#4754=LINE('',#26835,#5729);
#4755=LINE('',#26857,#5730);
#4756=LINE('',#26860,#5731);
#4757=LINE('',#26862,#5732);
#4758=LINE('',#26873,#5733);
#4759=LINE('',#26875,#5734);
#4760=LINE('',#26877,#5735);
#4761=LINE('',#26899,#5736);
#4762=LINE('',#26902,#5737);
#4763=LINE('',#26904,#5738);
#4764=LINE('',#26915,#5739);
#4765=LINE('',#26917,#5740);
#4766=LINE('',#26919,#5741);
#4767=LINE('',#26941,#5742);
#4768=LINE('',#26944,#5743);
#4769=LINE('',#26946,#5744);
#4770=LINE('',#26957,#5745);
#4771=LINE('',#26959,#5746);
#4772=LINE('',#26961,#5747);
#4773=LINE('',#26983,#5748);
#4774=LINE('',#26986,#5749);
#4775=LINE('',#26988,#5750);
#4776=LINE('',#26999,#5751);
#4777=LINE('',#27001,#5752);
#4778=LINE('',#27003,#5753);
#4779=LINE('',#27025,#5754);
#4780=LINE('',#27033,#5755);
#4781=LINE('',#27035,#5756);
#4782=LINE('',#27036,#5757);
#4783=LINE('',#27041,#5758);
#4784=LINE('',#27052,#5759);
#4785=LINE('',#27056,#5760);
#4786=LINE('',#27058,#5761);
#4787=LINE('',#27063,#5762);
#4788=LINE('',#27082,#5763);
#4789=LINE('',#27085,#5764);
#4790=LINE('',#27087,#5765);
#4791=LINE('',#27094,#5766);
#4792=LINE('',#27096,#5767);
#4793=LINE('',#27105,#5768);
#4794=LINE('',#27124,#5769);
#4795=LINE('',#27128,#5770);
#4796=LINE('',#27130,#5771);
#4797=LINE('',#27132,#5772);
#4798=LINE('',#27171,#5773);
#4799=LINE('',#27172,#5774);
#4800=LINE('',#27186,#5775);
#4801=LINE('',#27188,#5776);
#4802=LINE('',#27190,#5777);
#4803=LINE('',#27212,#5778);
#4804=LINE('',#27215,#5779);
#4805=LINE('',#27217,#5780);
#4806=LINE('',#27228,#5781);
#4807=LINE('',#27230,#5782);
#4808=LINE('',#27232,#5783);
#4809=LINE('',#27254,#5784);
#4810=LINE('',#27257,#5785);
#4811=LINE('',#27259,#5786);
#4812=LINE('',#27270,#5787);
#4813=LINE('',#27272,#5788);
#4814=LINE('',#27274,#5789);
#4815=LINE('',#27296,#5790);
#4816=LINE('',#27299,#5791);
#4817=LINE('',#27301,#5792);
#4818=LINE('',#27312,#5793);
#4819=LINE('',#27314,#5794);
#4820=LINE('',#27316,#5795);
#4821=LINE('',#27338,#5796);
#4822=LINE('',#27341,#5797);
#4823=LINE('',#27343,#5798);
#4824=LINE('',#27354,#5799);
#4825=LINE('',#27356,#5800);
#4826=LINE('',#27358,#5801);
#4827=LINE('',#27380,#5802);
#4828=LINE('',#27383,#5803);
#4829=LINE('',#27385,#5804);
#4830=LINE('',#27396,#5805);
#4831=LINE('',#27398,#5806);
#4832=LINE('',#27400,#5807);
#4833=LINE('',#27422,#5808);
#4834=LINE('',#27425,#5809);
#4835=LINE('',#27427,#5810);
#4836=LINE('',#27438,#5811);
#4837=LINE('',#27440,#5812);
#4838=LINE('',#27442,#5813);
#4839=LINE('',#27464,#5814);
#4840=LINE('',#27467,#5815);
#4841=LINE('',#27469,#5816);
#4842=LINE('',#27480,#5817);
#4843=LINE('',#27482,#5818);
#4844=LINE('',#27484,#5819);
#4845=LINE('',#27506,#5820);
#4846=LINE('',#27514,#5821);
#4847=LINE('',#27516,#5822);
#4848=LINE('',#27517,#5823);
#4849=LINE('',#27522,#5824);
#4850=LINE('',#27533,#5825);
#4851=LINE('',#27537,#5826);
#4852=LINE('',#27539,#5827);
#4853=LINE('',#27544,#5828);
#4854=LINE('',#27563,#5829);
#4855=LINE('',#27567,#5830);
#4856=LINE('',#27569,#5831);
#4857=LINE('',#27571,#5832);
#4858=LINE('',#27614,#5833);
#4859=LINE('',#27615,#5834);
#4860=LINE('',#27621,#5835);
#4861=LINE('',#27623,#5836);
#4862=LINE('',#27627,#5837);
#4863=LINE('',#27642,#5838);
#4864=LINE('',#27645,#5839);
#4865=LINE('',#27647,#5840);
#4866=LINE('',#27654,#5841);
#4867=LINE('',#27656,#5842);
#4868=LINE('',#27665,#5843);
#4869=LINE('',#27684,#5844);
#4870=LINE('',#27687,#5845);
#4871=LINE('',#27689,#5846);
#4872=LINE('',#27696,#5847);
#4873=LINE('',#27698,#5848);
#4874=LINE('',#27707,#5849);
#4875=LINE('',#27726,#5850);
#4876=LINE('',#27729,#5851);
#4877=LINE('',#27731,#5852);
#4878=LINE('',#27738,#5853);
#4879=LINE('',#27740,#5854);
#4880=LINE('',#27749,#5855);
#4881=LINE('',#27768,#5856);
#4882=LINE('',#27771,#5857);
#4883=LINE('',#27773,#5858);
#4884=LINE('',#27780,#5859);
#4885=LINE('',#27782,#5860);
#4886=LINE('',#27791,#5861);
#4887=LINE('',#27810,#5862);
#4888=LINE('',#27813,#5863);
#4889=LINE('',#27815,#5864);
#4890=LINE('',#27822,#5865);
#4891=LINE('',#27824,#5866);
#4892=LINE('',#27833,#5867);
#4893=LINE('',#27852,#5868);
#4894=LINE('',#27855,#5869);
#4895=LINE('',#27857,#5870);
#4896=LINE('',#27864,#5871);
#4897=LINE('',#27866,#5872);
#4898=LINE('',#27875,#5873);
#4899=LINE('',#27894,#5874);
#4900=LINE('',#27897,#5875);
#4901=LINE('',#27899,#5876);
#4902=LINE('',#27906,#5877);
#4903=LINE('',#27908,#5878);
#4904=LINE('',#27917,#5879);
#4905=LINE('',#27936,#5880);
#4906=LINE('',#27939,#5881);
#4907=LINE('',#27941,#5882);
#4908=LINE('',#27948,#5883);
#4909=LINE('',#27950,#5884);
#4910=LINE('',#27959,#5885);
#4911=LINE('',#27978,#5886);
#4912=LINE('',#27981,#5887);
#4913=LINE('',#27986,#5888);
#4914=LINE('',#27991,#5889);
#4915=LINE('',#27998,#5890);
#4916=LINE('',#28034,#5891);
#4917=LINE('',#28038,#5892);
#4918=LINE('',#28041,#5893);
#4919=LINE('',#28042,#5894);
#4920=LINE('',#28079,#5895);
#4921=LINE('',#28081,#5896);
#4922=LINE('',#28082,#5897);
#4923=LINE('',#28087,#5898);
#4924=LINE('',#28089,#5899);
#4925=LINE('',#28108,#5900);
#4926=LINE('',#28110,#5901);
#4927=LINE('',#28111,#5902);
#4928=LINE('',#28116,#5903);
#4929=LINE('',#28124,#5904);
#4930=LINE('',#28126,#5905);
#4931=LINE('',#28128,#5906);
#4932=LINE('',#28146,#5907);
#4933=LINE('',#28147,#5908);
#4934=LINE('',#28155,#5909);
#4935=LINE('',#28159,#5910);
#4936=LINE('',#28161,#5911);
#4937=LINE('',#28180,#5912);
#4938=LINE('',#28182,#5913);
#4939=LINE('',#28183,#5914);
#4940=LINE('',#28188,#5915);
#4941=LINE('',#28196,#5916);
#4942=LINE('',#28198,#5917);
#4943=LINE('',#28200,#5918);
#4944=LINE('',#28218,#5919);
#4945=LINE('',#28219,#5920);
#4946=LINE('',#28227,#5921);
#4947=LINE('',#28231,#5922);
#4948=LINE('',#28233,#5923);
#4949=LINE('',#28252,#5924);
#4950=LINE('',#28254,#5925);
#4951=LINE('',#28255,#5926);
#4952=LINE('',#28260,#5927);
#4953=LINE('',#28267,#5928);
#4954=LINE('',#28269,#5929);
#4955=LINE('',#28283,#5930);
#4956=LINE('',#28284,#5931);
#4957=LINE('',#28289,#5932);
#4958=LINE('',#28296,#5933);
#4959=LINE('',#28402,#5934);
#4960=LINE('',#28419,#5935);
#4961=LINE('',#28423,#5936);
#4962=LINE('',#28427,#5937);
#4963=LINE('',#28431,#5938);
#4964=LINE('',#28435,#5939);
#4965=LINE('',#28439,#5940);
#4966=LINE('',#28443,#5941);
#4967=LINE('',#28447,#5942);
#4968=LINE('',#28451,#5943);
#4969=LINE('',#28455,#5944);
#4970=LINE('',#28458,#5945);
#4971=LINE('',#28575,#5946);
#4972=LINE('',#28580,#5947);
#4973=LINE('',#28585,#5948);
#4974=LINE('',#28590,#5949);
#4975=LINE('',#28595,#5950);
#4976=LINE('',#28598,#5951);
#4977=LINE('',#28605,#5952);
#4978=LINE('',#28674,#5953);
#4979=LINE('',#28761,#5954);
#4980=LINE('',#28851,#5955);
#4981=LINE('',#28938,#5956);
#4982=LINE('',#29025,#5957);
#4983=LINE('',#29115,#5958);
#4984=LINE('',#29202,#5959);
#4985=LINE('',#29289,#5960);
#4986=LINE('',#29379,#5961);
#4987=LINE('',#29466,#5962);
#4988=LINE('',#29553,#5963);
#4989=LINE('',#29583,#5964);
#4990=LINE('',#29616,#5965);
#4991=LINE('',#29653,#5966);
#4992=LINE('',#29691,#5967);
#4993=LINE('',#29728,#5968);
#4994=LINE('',#29765,#5969);
#4995=LINE('',#29803,#5970);
#4996=LINE('',#29840,#5971);
#4997=LINE('',#29877,#5972);
#4998=LINE('',#29915,#5973);
#4999=LINE('',#29952,#5974);
#5000=LINE('',#29989,#5975);
#5001=LINE('',#31884,#5976);
#5002=LINE('',#31891,#5977);
#5003=LINE('',#31895,#5978);
#5004=LINE('',#31901,#5979);
#5005=LINE('',#31925,#5980);
#5006=LINE('',#31973,#5981);
#5007=LINE('',#32024,#5982);
#5008=LINE('',#32075,#5983);
#5009=LINE('',#32123,#5984);
#5010=LINE('',#32177,#5985);
#5011=LINE('',#32195,#5986);
#5012=LINE('',#32220,#5987);
#5013=LINE('',#32245,#5988);
#5014=LINE('',#32269,#5989);
#5015=LINE('',#32295,#5990);
#5016=LINE('',#33108,#5991);
#5017=LINE('',#33112,#5992);
#5018=LINE('',#33117,#5993);
#5019=LINE('',#33126,#5994);
#5020=LINE('',#33132,#5995);
#5021=LINE('',#33137,#5996);
#5022=LINE('',#33145,#5997);
#5023=LINE('',#33149,#5998);
#5024=LINE('',#33156,#5999);
#5025=LINE('',#33162,#6000);
#5026=LINE('',#33170,#6001);
#5027=LINE('',#33178,#6002);
#5028=LINE('',#33185,#6003);
#5029=LINE('',#33191,#6004);
#5030=LINE('',#33198,#6005);
#5031=LINE('',#33204,#6006);
#5032=LINE('',#33210,#6007);
#5033=LINE('',#33214,#6008);
#5034=LINE('',#33222,#6009);
#5035=LINE('',#33228,#6010);
#5036=LINE('',#33615,#6011);
#5037=LINE('',#33624,#6012);
#5038=LINE('',#33626,#6013);
#5039=LINE('',#33642,#6014);
#5040=LINE('',#33645,#6015);
#5041=LINE('',#33667,#6016);
#5042=LINE('',#33699,#6017);
#5043=LINE('',#33700,#6018);
#5044=LINE('',#33732,#6019);
#5045=LINE('',#33733,#6020);
#5046=LINE('',#33740,#6021);
#5047=LINE('',#33741,#6022);
#5048=LINE('',#33773,#6023);
#5049=LINE('',#33774,#6024);
#5050=LINE('',#33781,#6025);
#5051=LINE('',#33782,#6026);
#5052=LINE('',#33789,#6027);
#5053=LINE('',#33790,#6028);
#5054=LINE('',#33805,#6029);
#5055=LINE('',#34593,#6030);
#5056=LINE('',#34617,#6031);
#5057=LINE('',#34665,#6032);
#5058=LINE('',#34713,#6033);
#5059=LINE('',#34761,#6034);
#5060=LINE('',#34780,#6035);
#5061=LINE('',#34805,#6036);
#5062=LINE('',#34829,#6037);
#5063=LINE('',#35525,#6038);
#5064=LINE('',#35527,#6039);
#5065=LINE('',#35529,#6040);
#5066=LINE('',#35530,#6041);
#5067=LINE('',#35533,#6042);
#5068=LINE('',#35535,#6043);
#5069=LINE('',#35536,#6044);
#5070=LINE('',#35539,#6045);
#5071=LINE('',#35541,#6046);
#5072=LINE('',#35542,#6047);
#5073=LINE('',#35545,#6048);
#5074=LINE('',#35547,#6049);
#5075=LINE('',#35548,#6050);
#5076=LINE('',#35551,#6051);
#5077=LINE('',#35553,#6052);
#5078=LINE('',#35554,#6053);
#5079=LINE('',#35556,#6054);
#5080=LINE('',#35557,#6055);
#5081=LINE('',#35563,#6056);
#5082=LINE('',#35569,#6057);
#5083=LINE('',#35575,#6058);
#5084=LINE('',#35599,#6059);
#5085=LINE('',#35647,#6060);
#5086=LINE('',#35695,#6061);
#5087=LINE('',#35749,#6062);
#5088=LINE('',#35797,#6063);
#5089=LINE('',#35845,#6064);
#5090=LINE('',#35893,#6065);
#5091=LINE('',#35947,#6066);
#5092=LINE('',#35995,#6067);
#5093=LINE('',#36043,#6068);
#5094=LINE('',#36097,#6069);
#5095=LINE('',#36145,#6070);
#5096=LINE('',#36193,#6071);
#5097=LINE('',#36247,#6072);
#5098=LINE('',#36295,#6073);
#5099=LINE('',#36319,#6074);
#5100=LINE('',#36344,#6075);
#5101=LINE('',#36369,#6076);
#5102=LINE('',#36393,#6077);
#5103=LINE('',#36418,#6078);
#5104=LINE('',#36443,#6079);
#5105=LINE('',#36467,#6080);
#5106=LINE('',#36492,#6081);
#5107=LINE('',#36517,#6082);
#5108=LINE('',#36541,#6083);
#5109=LINE('',#36565,#6084);
#5110=LINE('',#36590,#6085);
#5111=LINE('',#36615,#6086);
#5112=LINE('',#37809,#6087);
#5113=LINE('',#37811,#6088);
#5114=LINE('',#37812,#6089);
#5115=LINE('',#37816,#6090);
#5116=LINE('',#37822,#6091);
#5117=LINE('',#37827,#6092);
#5118=LINE('',#37831,#6093);
#5119=LINE('',#37835,#6094);
#5120=LINE('',#37839,#6095);
#5121=LINE('',#37843,#6096);
#5122=LINE('',#37847,#6097);
#5123=LINE('',#37851,#6098);
#5124=LINE('',#37855,#6099);
#5125=LINE('',#37859,#6100);
#5126=LINE('',#37863,#6101);
#5127=LINE('',#37867,#6102);
#5128=LINE('',#37871,#6103);
#5129=LINE('',#37875,#6104);
#5130=LINE('',#37879,#6105);
#5131=LINE('',#37883,#6106);
#5132=LINE('',#37887,#6107);
#5133=LINE('',#37891,#6108);
#5134=LINE('',#37895,#6109);
#5135=LINE('',#37899,#6110);
#5136=LINE('',#37903,#6111);
#5137=LINE('',#37907,#6112);
#5138=LINE('',#37911,#6113);
#5139=LINE('',#37915,#6114);
#5140=LINE('',#37919,#6115);
#5141=LINE('',#37923,#6116);
#5142=LINE('',#37927,#6117);
#5143=LINE('',#37931,#6118);
#5144=LINE('',#37935,#6119);
#5145=LINE('',#37940,#6120);
#5146=LINE('',#37944,#6121);
#5147=LINE('',#37948,#6122);
#5148=LINE('',#37952,#6123);
#5149=LINE('',#37956,#6124);
#5150=LINE('',#37960,#6125);
#5151=LINE('',#37964,#6126);
#5152=LINE('',#37968,#6127);
#5153=LINE('',#37972,#6128);
#5154=LINE('',#37976,#6129);
#5155=LINE('',#37980,#6130);
#5156=LINE('',#37984,#6131);
#5157=LINE('',#37988,#6132);
#5158=LINE('',#37992,#6133);
#5159=LINE('',#37996,#6134);
#5160=LINE('',#38000,#6135);
#5161=LINE('',#38004,#6136);
#5162=LINE('',#38008,#6137);
#5163=LINE('',#38012,#6138);
#5164=LINE('',#38016,#6139);
#5165=LINE('',#38020,#6140);
#5166=LINE('',#38024,#6141);
#5167=LINE('',#38028,#6142);
#5168=LINE('',#38032,#6143);
#5169=LINE('',#38036,#6144);
#5170=LINE('',#38040,#6145);
#5171=LINE('',#38044,#6146);
#5172=LINE('',#38048,#6147);
#5173=LINE('',#38052,#6148);
#5174=LINE('',#38056,#6149);
#5175=LINE('',#38060,#6150);
#5176=LINE('',#38068,#6151);
#5177=LINE('',#38069,#6152);
#5178=LINE('',#38071,#6153);
#5179=LINE('',#38082,#6154);
#5180=LINE('',#38083,#6155);
#5181=LINE('',#38085,#6156);
#5182=LINE('',#38096,#6157);
#5183=LINE('',#38097,#6158);
#5184=LINE('',#38099,#6159);
#5185=LINE('',#38110,#6160);
#5186=LINE('',#38111,#6161);
#5187=LINE('',#38113,#6162);
#5188=LINE('',#38124,#6163);
#5189=LINE('',#38125,#6164);
#5190=LINE('',#38127,#6165);
#5191=LINE('',#38138,#6166);
#5192=LINE('',#38139,#6167);
#5193=LINE('',#38141,#6168);
#5194=LINE('',#38152,#6169);
#5195=LINE('',#38153,#6170);
#5196=LINE('',#38155,#6171);
#5197=LINE('',#38166,#6172);
#5198=LINE('',#38167,#6173);
#5199=LINE('',#38169,#6174);
#5200=LINE('',#38180,#6175);
#5201=LINE('',#38181,#6176);
#5202=LINE('',#38183,#6177);
#5203=LINE('',#38194,#6178);
#5204=LINE('',#38195,#6179);
#5205=LINE('',#38197,#6180);
#5206=LINE('',#38208,#6181);
#5207=LINE('',#38209,#6182);
#5208=LINE('',#38211,#6183);
#5209=LINE('',#38222,#6184);
#5210=LINE('',#38223,#6185);
#5211=LINE('',#38225,#6186);
#5212=LINE('',#38236,#6187);
#5213=LINE('',#38237,#6188);
#5214=LINE('',#38239,#6189);
#5215=LINE('',#38250,#6190);
#5216=LINE('',#38251,#6191);
#5217=LINE('',#38253,#6192);
#5218=LINE('',#38264,#6193);
#5219=LINE('',#38265,#6194);
#5220=LINE('',#38267,#6195);
#5221=LINE('',#38278,#6196);
#5222=LINE('',#38279,#6197);
#5223=LINE('',#38281,#6198);
#5224=LINE('',#38292,#6199);
#5225=LINE('',#38293,#6200);
#5226=LINE('',#38295,#6201);
#5227=LINE('',#38306,#6202);
#5228=LINE('',#38307,#6203);
#5229=LINE('',#38309,#6204);
#5230=LINE('',#38320,#6205);
#5231=LINE('',#38321,#6206);
#5232=LINE('',#38323,#6207);
#5233=LINE('',#38334,#6208);
#5234=LINE('',#38335,#6209);
#5235=LINE('',#38337,#6210);
#5236=LINE('',#38348,#6211);
#5237=LINE('',#38349,#6212);
#5238=LINE('',#38351,#6213);
#5239=LINE('',#38362,#6214);
#5240=LINE('',#38363,#6215);
#5241=LINE('',#38365,#6216);
#5242=LINE('',#38376,#6217);
#5243=LINE('',#38377,#6218);
#5244=LINE('',#38379,#6219);
#5245=LINE('',#38390,#6220);
#5246=LINE('',#38391,#6221);
#5247=LINE('',#38393,#6222);
#5248=LINE('',#38404,#6223);
#5249=LINE('',#38405,#6224);
#5250=LINE('',#38407,#6225);
#5251=LINE('',#38418,#6226);
#5252=LINE('',#38419,#6227);
#5253=LINE('',#38421,#6228);
#5254=LINE('',#38432,#6229);
#5255=LINE('',#38433,#6230);
#5256=LINE('',#38435,#6231);
#5257=LINE('',#38446,#6232);
#5258=LINE('',#38447,#6233);
#5259=LINE('',#38449,#6234);
#5260=LINE('',#38460,#6235);
#5261=LINE('',#38461,#6236);
#5262=LINE('',#38463,#6237);
#5263=LINE('',#38472,#6238);
#5264=LINE('',#38479,#6239);
#5265=LINE('',#38483,#6240);
#5266=VECTOR('',#19031,10.);
#5267=VECTOR('',#19032,10.);
#5268=VECTOR('',#19033,10.);
#5269=VECTOR('',#19034,10.);
#5270=VECTOR('',#19037,10.);
#5271=VECTOR('',#19038,10.);
#5272=VECTOR('',#19039,10.);
#5273=VECTOR('',#19040,10.);
#5274=VECTOR('',#19043,10.);
#5275=VECTOR('',#19044,10.);
#5276=VECTOR('',#19047,10.);
#5277=VECTOR('',#19048,10.);
#5278=VECTOR('',#19051,10.);
#5279=VECTOR('',#19052,10.);
#5280=VECTOR('',#19053,10.);
#5281=VECTOR('',#19056,10.);
#5282=VECTOR('',#19057,10.);
#5283=VECTOR('',#19060,10.);
#5284=VECTOR('',#19061,10.);
#5285=VECTOR('',#19062,10.);
#5286=VECTOR('',#19067,10.);
#5287=VECTOR('',#19068,10.);
#5288=VECTOR('',#19069,10.);
#5289=VECTOR('',#19070,10.);
#5290=VECTOR('',#19071,10.);
#5291=VECTOR('',#19072,10.);
#5292=VECTOR('',#19073,10.);
#5293=VECTOR('',#19074,10.);
#5294=VECTOR('',#19075,10.);
#5295=VECTOR('',#19076,10.);
#5296=VECTOR('',#19077,10.);
#5297=VECTOR('',#19078,10.);
#5298=VECTOR('',#19081,10.);
#5299=VECTOR('',#19082,10.);
#5300=VECTOR('',#19083,10.);
#5301=VECTOR('',#19086,10.);
#5302=VECTOR('',#19087,10.);
#5303=VECTOR('',#19090,10.);
#5304=VECTOR('',#19091,10.);
#5305=VECTOR('',#19094,10.);
#5306=VECTOR('',#19095,10.);
#5307=VECTOR('',#19096,10.);
#5308=VECTOR('',#19099,10.);
#5309=VECTOR('',#19100,10.);
#5310=VECTOR('',#19103,10.);
#5311=VECTOR('',#19104,10.);
#5312=VECTOR('',#19107,10.);
#5313=VECTOR('',#19108,10.);
#5314=VECTOR('',#19109,10.);
#5315=VECTOR('',#19112,10.);
#5316=VECTOR('',#19113,10.);
#5317=VECTOR('',#19114,10.);
#5318=VECTOR('',#19117,10.);
#5319=VECTOR('',#19118,10.);
#5320=VECTOR('',#19119,10.);
#5321=VECTOR('',#19122,10.);
#5322=VECTOR('',#19123,10.);
#5323=VECTOR('',#19124,10.);
#5324=VECTOR('',#19127,10.);
#5325=VECTOR('',#19128,10.);
#5326=VECTOR('',#19129,10.);
#5327=VECTOR('',#19132,10.);
#5328=VECTOR('',#19133,10.);
#5329=VECTOR('',#19134,10.);
#5330=VECTOR('',#19137,10.);
#5331=VECTOR('',#19138,10.);
#5332=VECTOR('',#19139,10.);
#5333=VECTOR('',#19142,10.);
#5334=VECTOR('',#19143,10.);
#5335=VECTOR('',#19144,10.);
#5336=VECTOR('',#19147,10.);
#5337=VECTOR('',#19148,10.);
#5338=VECTOR('',#19149,10.);
#5339=VECTOR('',#19154,10.);
#5340=VECTOR('',#19157,10.);
#5341=VECTOR('',#19158,10.);
#5342=VECTOR('',#19159,10.);
#5343=VECTOR('',#19164,10.);
#5344=VECTOR('',#19167,10.);
#5345=VECTOR('',#19168,10.);
#5346=VECTOR('',#19169,10.);
#5347=VECTOR('',#19170,10.);
#5348=VECTOR('',#19173,10.);
#5349=VECTOR('',#19176,10.);
#5350=VECTOR('',#19177,10.);
#5351=VECTOR('',#19178,10.);
#5352=VECTOR('',#19179,10.);
#5353=VECTOR('',#19182,10.);
#5354=VECTOR('',#19187,10.);
#5355=VECTOR('',#19188,10.);
#5356=VECTOR('',#19199,10.);
#5357=VECTOR('',#19206,10.);
#5358=VECTOR('',#19209,10.);
#5359=VECTOR('',#19210,10.);
#5360=VECTOR('',#19213,10.);
#5361=VECTOR('',#19226,10.);
#5362=VECTOR('',#19229,10.);
#5363=VECTOR('',#19232,10.);
#5364=VECTOR('',#19235,10.);
#5365=VECTOR('',#19238,10.);
#5366=VECTOR('',#19241,10.);
#5367=VECTOR('',#19244,10.);
#5368=VECTOR('',#19247,10.);
#5369=VECTOR('',#19250,10.);
#5370=VECTOR('',#19253,10.);
#5371=VECTOR('',#19256,2.8);
#5372=VECTOR('',#19261,2.55);
#5373=VECTOR('',#19266,10.);
#5374=VECTOR('',#19267,10.);
#5375=VECTOR('',#19274,10.);
#5376=VECTOR('',#19279,10.);
#5377=VECTOR('',#19288,47.8232233047034);
#5378=VECTOR('',#19295,47.6);
#5379=VECTOR('',#19298,48.);
#5380=VECTOR('',#19301,11.25);
#5381=VECTOR('',#19308,11.);
#5382=VECTOR('',#19311,47.1267766952966);
#5383=VECTOR('',#19324,11.3);
#5384=VECTOR('',#19327,2.55);
#5385=VECTOR('',#19338,2.05);
#5386=VECTOR('',#19341,5.);
#5387=VECTOR('',#19354,10.);
#5388=VECTOR('',#19355,10.);
#5389=VECTOR('',#19358,10.);
#5390=VECTOR('',#19365,10.);
#5391=VECTOR('',#19366,10.);
#5392=VECTOR('',#19367,10.);
#5393=VECTOR('',#19372,10.);
#5394=VECTOR('',#19381,10.);
#5395=VECTOR('',#19382,10.);
#5396=VECTOR('',#19383,10.);
#5397=VECTOR('',#19388,10.);
#5398=VECTOR('',#19397,10.);
#5399=VECTOR('',#19398,10.);
#5400=VECTOR('',#19403,10.);
#5401=VECTOR('',#19408,10.);
#5402=VECTOR('',#19409,10.);
#5403=VECTOR('',#19410,10.);
#5404=VECTOR('',#19421,10.);
#5405=VECTOR('',#19424,10.);
#5406=VECTOR('',#19425,10.);
#5407=VECTOR('',#19426,10.);
#5408=VECTOR('',#19439,10.);
#5409=VECTOR('',#19440,10.);
#5410=VECTOR('',#19441,10.);
#5411=VECTOR('',#19452,10.);
#5412=VECTOR('',#19455,10.);
#5413=VECTOR('',#19456,10.);
#5414=VECTOR('',#19459,10.);
#5415=VECTOR('',#19460,10.);
#5416=VECTOR('',#19463,10.);
#5417=VECTOR('',#19464,10.);
#5418=VECTOR('',#19465,10.);
#5419=VECTOR('',#19470,10.);
#5420=VECTOR('',#19481,10.);
#5421=VECTOR('',#19482,10.);
#5422=VECTOR('',#19483,10.);
#5423=VECTOR('',#19488,10.);
#5424=VECTOR('',#19497,10.);
#5425=VECTOR('',#19498,10.);
#5426=VECTOR('',#19499,10.);
#5427=VECTOR('',#19510,10.);
#5428=VECTOR('',#19513,10.);
#5429=VECTOR('',#19514,10.);
#5430=VECTOR('',#19517,10.);
#5431=VECTOR('',#19518,10.);
#5432=VECTOR('',#19519,10.);
#5433=VECTOR('',#19530,10.);
#5434=VECTOR('',#19533,10.);
#5435=VECTOR('',#19534,10.);
#5436=VECTOR('',#19537,10.);
#5437=VECTOR('',#19538,10.);
#5438=VECTOR('',#19539,10.);
#5439=VECTOR('',#19550,10.);
#5440=VECTOR('',#19553,10.);
#5441=VECTOR('',#19554,10.);
#5442=VECTOR('',#19557,10.);
#5443=VECTOR('',#19558,10.);
#5444=VECTOR('',#19559,10.);
#5445=VECTOR('',#19570,10.);
#5446=VECTOR('',#19573,10.);
#5447=VECTOR('',#19574,10.);
#5448=VECTOR('',#19577,10.);
#5449=VECTOR('',#19578,10.);
#5450=VECTOR('',#19579,10.);
#5451=VECTOR('',#19590,10.);
#5452=VECTOR('',#19593,10.);
#5453=VECTOR('',#19594,10.);
#5454=VECTOR('',#19597,10.);
#5455=VECTOR('',#19598,10.);
#5456=VECTOR('',#19599,10.);
#5457=VECTOR('',#19610,10.);
#5458=VECTOR('',#19613,10.);
#5459=VECTOR('',#19614,10.);
#5460=VECTOR('',#19617,10.);
#5461=VECTOR('',#19618,10.);
#5462=VECTOR('',#19619,10.);
#5463=VECTOR('',#19630,10.);
#5464=VECTOR('',#19633,10.);
#5465=VECTOR('',#19634,10.);
#5466=VECTOR('',#19637,10.);
#5467=VECTOR('',#19638,10.);
#5468=VECTOR('',#19639,10.);
#5469=VECTOR('',#19650,10.);
#5470=VECTOR('',#19653,10.);
#5471=VECTOR('',#19654,10.);
#5472=VECTOR('',#20003,10.);
#5473=VECTOR('',#20006,10.);
#5474=VECTOR('',#20009,10.);
#5475=VECTOR('',#20010,10.);
#5476=VECTOR('',#20013,10.);
#5477=VECTOR('',#20014,10.);
#5478=VECTOR('',#20015,10.);
#5479=VECTOR('',#20024,10.);
#5480=VECTOR('',#20027,10.);
#5481=VECTOR('',#20028,10.);
#5482=VECTOR('',#20031,10.);
#5483=VECTOR('',#20032,10.);
#5484=VECTOR('',#20033,10.);
#5485=VECTOR('',#20042,10.);
#5486=VECTOR('',#20045,10.);
#5487=VECTOR('',#20046,10.);
#5488=VECTOR('',#20049,10.);
#5489=VECTOR('',#20050,10.);
#5490=VECTOR('',#20051,10.);
#5491=VECTOR('',#20060,10.);
#5492=VECTOR('',#20063,10.);
#5493=VECTOR('',#20064,10.);
#5494=VECTOR('',#20069,10.);
#5495=VECTOR('',#20076,10.);
#5496=VECTOR('',#20079,10.);
#5497=VECTOR('',#20080,10.);
#5498=VECTOR('',#20081,10.);
#5499=VECTOR('',#20090,10.);
#5500=VECTOR('',#20093,10.);
#5501=VECTOR('',#20094,10.);
#5502=VECTOR('',#20097,10.);
#5503=VECTOR('',#20098,10.);
#5504=VECTOR('',#20099,10.);
#5505=VECTOR('',#20108,10.);
#5506=VECTOR('',#20111,10.);
#5507=VECTOR('',#20112,10.);
#5508=VECTOR('',#20115,10.);
#5509=VECTOR('',#20116,10.);
#5510=VECTOR('',#20117,10.);
#5511=VECTOR('',#20126,10.);
#5512=VECTOR('',#20129,10.);
#5513=VECTOR('',#20130,10.);
#5514=VECTOR('',#20133,10.);
#5515=VECTOR('',#20134,10.);
#5516=VECTOR('',#20135,10.);
#5517=VECTOR('',#20144,10.);
#5518=VECTOR('',#20147,10.);
#5519=VECTOR('',#20148,10.);
#5520=VECTOR('',#20151,10.);
#5521=VECTOR('',#20152,10.);
#5522=VECTOR('',#20153,10.);
#5523=VECTOR('',#20162,10.);
#5524=VECTOR('',#20165,10.);
#5525=VECTOR('',#20166,10.);
#5526=VECTOR('',#20169,10.);
#5527=VECTOR('',#20170,10.);
#5528=VECTOR('',#20171,10.);
#5529=VECTOR('',#20180,10.);
#5530=VECTOR('',#20183,10.);
#5531=VECTOR('',#20184,10.);
#5532=VECTOR('',#20185,10.);
#5533=VECTOR('',#20212,10.);
#5534=VECTOR('',#20213,10.);
#5535=VECTOR('',#20260,10.);
#5536=VECTOR('',#20261,10.);
#5537=VECTOR('',#20262,10.);
#5538=VECTOR('',#20271,10.);
#5539=VECTOR('',#20274,10.);
#5540=VECTOR('',#20275,10.);
#5541=VECTOR('',#20282,10.);
#5542=VECTOR('',#20283,10.);
#5543=VECTOR('',#20284,10.);
#5544=VECTOR('',#20293,10.);
#5545=VECTOR('',#20296,10.);
#5546=VECTOR('',#20297,10.);
#5547=VECTOR('',#20300,10.);
#5548=VECTOR('',#20301,10.);
#5549=VECTOR('',#20302,10.);
#5550=VECTOR('',#20311,10.);
#5551=VECTOR('',#20314,10.);
#5552=VECTOR('',#20315,10.);
#5553=VECTOR('',#20318,10.);
#5554=VECTOR('',#20319,10.);
#5555=VECTOR('',#20320,10.);
#5556=VECTOR('',#20329,10.);
#5557=VECTOR('',#20332,10.);
#5558=VECTOR('',#20333,10.);
#5559=VECTOR('',#20334,10.);
#5560=VECTOR('',#20339,10.);
#5561=VECTOR('',#20346,10.);
#5562=VECTOR('',#20349,10.);
#5563=VECTOR('',#20350,10.);
#5564=VECTOR('',#20351,10.);
#5565=VECTOR('',#20360,10.);
#5566=VECTOR('',#20363,10.);
#5567=VECTOR('',#20364,10.);
#5568=VECTOR('',#20367,10.);
#5569=VECTOR('',#20368,10.);
#5570=VECTOR('',#20369,10.);
#5571=VECTOR('',#20378,10.);
#5572=VECTOR('',#20381,10.);
#5573=VECTOR('',#20382,10.);
#5574=VECTOR('',#20385,10.);
#5575=VECTOR('',#20386,10.);
#5576=VECTOR('',#20387,10.);
#5577=VECTOR('',#20396,10.);
#5578=VECTOR('',#20399,10.);
#5579=VECTOR('',#20400,10.);
#5580=VECTOR('',#20403,10.);
#5581=VECTOR('',#20404,10.);
#5582=VECTOR('',#20405,10.);
#5583=VECTOR('',#20414,10.);
#5584=VECTOR('',#20417,10.);
#5585=VECTOR('',#20418,10.);
#5586=VECTOR('',#20421,10.);
#5587=VECTOR('',#20422,10.);
#5588=VECTOR('',#20423,10.);
#5589=VECTOR('',#20432,10.);
#5590=VECTOR('',#20435,10.);
#5591=VECTOR('',#20436,10.);
#5592=VECTOR('',#20437,10.);
#5593=VECTOR('',#20468,10.);
#5594=VECTOR('',#20469,10.);
#5595=VECTOR('',#20508,10.);
#5596=VECTOR('',#20509,10.);
#5597=VECTOR('',#20510,10.);
#5598=VECTOR('',#20519,10.);
#5599=VECTOR('',#20522,10.);
#5600=VECTOR('',#20523,10.);
#5601=VECTOR('',#20526,10.);
#5602=VECTOR('',#20527,10.);
#5603=VECTOR('',#20528,10.);
#5604=VECTOR('',#20537,10.);
#5605=VECTOR('',#20540,10.);
#5606=VECTOR('',#20541,10.);
#5607=VECTOR('',#20544,10.);
#5608=VECTOR('',#20545,10.);
#5609=VECTOR('',#20546,10.);
#5610=VECTOR('',#20555,10.);
#5611=VECTOR('',#20558,10.);
#5612=VECTOR('',#20559,10.);
#5613=VECTOR('',#20562,10.);
#5614=VECTOR('',#20563,10.);
#5615=VECTOR('',#20564,10.);
#5616=VECTOR('',#20573,10.);
#5617=VECTOR('',#20576,10.);
#5618=VECTOR('',#20577,10.);
#5619=VECTOR('',#20580,10.);
#5620=VECTOR('',#20581,10.);
#5621=VECTOR('',#20582,10.);
#5622=VECTOR('',#20591,10.);
#5623=VECTOR('',#20594,10.);
#5624=VECTOR('',#20595,10.);
#5625=VECTOR('',#20596,10.);
#5626=VECTOR('',#20601,10.);
#5627=VECTOR('',#20608,10.);
#5628=VECTOR('',#20611,10.);
#5629=VECTOR('',#20612,10.);
#5630=VECTOR('',#20613,10.);
#5631=VECTOR('',#20622,10.);
#5632=VECTOR('',#20625,10.);
#5633=VECTOR('',#20626,10.);
#5634=VECTOR('',#20629,10.);
#5635=VECTOR('',#20630,10.);
#5636=VECTOR('',#20631,10.);
#5637=VECTOR('',#20640,10.);
#5638=VECTOR('',#20643,10.);
#5639=VECTOR('',#20644,10.);
#5640=VECTOR('',#20647,10.);
#5641=VECTOR('',#20648,10.);
#5642=VECTOR('',#20649,10.);
#5643=VECTOR('',#20658,10.);
#5644=VECTOR('',#20661,10.);
#5645=VECTOR('',#20662,10.);
#5646=VECTOR('',#20665,10.);
#5647=VECTOR('',#20666,10.);
#5648=VECTOR('',#20667,10.);
#5649=VECTOR('',#20676,10.);
#5650=VECTOR('',#20679,10.);
#5651=VECTOR('',#20680,10.);
#5652=VECTOR('',#20681,10.);
#5653=VECTOR('',#20724,10.);
#5654=VECTOR('',#20725,10.);
#5655=VECTOR('',#20756,10.);
#5656=VECTOR('',#20757,10.);
#5657=VECTOR('',#20758,10.);
#5658=VECTOR('',#20767,10.);
#5659=VECTOR('',#20770,10.);
#5660=VECTOR('',#20771,10.);
#5661=VECTOR('',#20778,10.);
#5662=VECTOR('',#20779,10.);
#5663=VECTOR('',#20780,10.);
#5664=VECTOR('',#20789,10.);
#5665=VECTOR('',#20792,10.);
#5666=VECTOR('',#20793,10.);
#5667=VECTOR('',#20796,10.);
#5668=VECTOR('',#20797,10.);
#5669=VECTOR('',#20798,10.);
#5670=VECTOR('',#20807,10.);
#5671=VECTOR('',#20810,10.);
#5672=VECTOR('',#20811,10.);
#5673=VECTOR('',#20814,10.);
#5674=VECTOR('',#20815,10.);
#5675=VECTOR('',#20816,10.);
#5676=VECTOR('',#20825,10.);
#5677=VECTOR('',#20828,10.);
#5678=VECTOR('',#20829,10.);
#5679=VECTOR('',#20832,10.);
#5680=VECTOR('',#20833,10.);
#5681=VECTOR('',#20834,10.);
#5682=VECTOR('',#20843,10.);
#5683=VECTOR('',#20846,10.);
#5684=VECTOR('',#20847,10.);
#5685=VECTOR('',#20850,10.);
#5686=VECTOR('',#20851,10.);
#5687=VECTOR('',#20852,10.);
#5688=VECTOR('',#20861,10.);
#5689=VECTOR('',#20864,10.);
#5690=VECTOR('',#20865,10.);
#5691=VECTOR('',#20866,10.);
#5692=VECTOR('',#20871,10.);
#5693=VECTOR('',#20878,10.);
#5694=VECTOR('',#20881,10.);
#5695=VECTOR('',#20882,10.);
#5696=VECTOR('',#20883,10.);
#5697=VECTOR('',#20892,10.);
#5698=VECTOR('',#20895,10.);
#5699=VECTOR('',#20896,10.);
#5700=VECTOR('',#20899,10.);
#5701=VECTOR('',#20900,10.);
#5702=VECTOR('',#20901,10.);
#5703=VECTOR('',#20910,10.);
#5704=VECTOR('',#20913,10.);
#5705=VECTOR('',#20914,10.);
#5706=VECTOR('',#20917,10.);
#5707=VECTOR('',#20918,10.);
#5708=VECTOR('',#20919,10.);
#5709=VECTOR('',#20928,10.);
#5710=VECTOR('',#20931,10.);
#5711=VECTOR('',#20932,10.);
#5712=VECTOR('',#20933,10.);
#5713=VECTOR('',#20980,10.);
#5714=VECTOR('',#20981,10.);
#5715=VECTOR('',#21004,10.);
#5716=VECTOR('',#21005,10.);
#5717=VECTOR('',#21006,10.);
#5718=VECTOR('',#21015,10.);
#5719=VECTOR('',#21018,10.);
#5720=VECTOR('',#21019,10.);
#5721=VECTOR('',#21022,10.);
#5722=VECTOR('',#21023,10.);
#5723=VECTOR('',#21024,10.);
#5724=VECTOR('',#21033,10.);
#5725=VECTOR('',#21036,10.);
#5726=VECTOR('',#21037,10.);
#5727=VECTOR('',#21040,10.);
#5728=VECTOR('',#21041,10.);
#5729=VECTOR('',#21042,10.);
#5730=VECTOR('',#21051,10.);
#5731=VECTOR('',#21054,10.);
#5732=VECTOR('',#21055,10.);
#5733=VECTOR('',#21058,10.);
#5734=VECTOR('',#21059,10.);
#5735=VECTOR('',#21060,10.);
#5736=VECTOR('',#21069,10.);
#5737=VECTOR('',#21072,10.);
#5738=VECTOR('',#21073,10.);
#5739=VECTOR('',#21076,10.);
#5740=VECTOR('',#21077,10.);
#5741=VECTOR('',#21078,10.);
#5742=VECTOR('',#21087,10.);
#5743=VECTOR('',#21090,10.);
#5744=VECTOR('',#21091,10.);
#5745=VECTOR('',#21094,10.);
#5746=VECTOR('',#21095,10.);
#5747=VECTOR('',#21096,10.);
#5748=VECTOR('',#21105,10.);
#5749=VECTOR('',#21108,10.);
#5750=VECTOR('',#21109,10.);
#5751=VECTOR('',#21112,10.);
#5752=VECTOR('',#21113,10.);
#5753=VECTOR('',#21114,10.);
#5754=VECTOR('',#21123,10.);
#5755=VECTOR('',#21126,10.);
#5756=VECTOR('',#21127,10.);
#5757=VECTOR('',#21128,10.);
#5758=VECTOR('',#21133,10.);
#5759=VECTOR('',#21140,10.);
#5760=VECTOR('',#21143,10.);
#5761=VECTOR('',#21144,10.);
#5762=VECTOR('',#21145,10.);
#5763=VECTOR('',#21154,10.);
#5764=VECTOR('',#21157,10.);
#5765=VECTOR('',#21158,10.);
#5766=VECTOR('',#21161,10.);
#5767=VECTOR('',#21162,10.);
#5768=VECTOR('',#21163,10.);
#5769=VECTOR('',#21172,10.);
#5770=VECTOR('',#21175,10.);
#5771=VECTOR('',#21176,10.);
#5772=VECTOR('',#21177,10.);
#5773=VECTOR('',#21236,10.);
#5774=VECTOR('',#21237,10.);
#5775=VECTOR('',#21252,10.);
#5776=VECTOR('',#21253,10.);
#5777=VECTOR('',#21254,10.);
#5778=VECTOR('',#21263,10.);
#5779=VECTOR('',#21266,10.);
#5780=VECTOR('',#21267,10.);
#5781=VECTOR('',#21270,10.);
#5782=VECTOR('',#21271,10.);
#5783=VECTOR('',#21272,10.);
#5784=VECTOR('',#21281,10.);
#5785=VECTOR('',#21284,10.);
#5786=VECTOR('',#21285,10.);
#5787=VECTOR('',#21288,10.);
#5788=VECTOR('',#21289,10.);
#5789=VECTOR('',#21290,10.);
#5790=VECTOR('',#21299,10.);
#5791=VECTOR('',#21302,10.);
#5792=VECTOR('',#21303,10.);
#5793=VECTOR('',#21306,10.);
#5794=VECTOR('',#21307,10.);
#5795=VECTOR('',#21308,10.);
#5796=VECTOR('',#21317,10.);
#5797=VECTOR('',#21320,10.);
#5798=VECTOR('',#21321,10.);
#5799=VECTOR('',#21324,10.);
#5800=VECTOR('',#21325,10.);
#5801=VECTOR('',#21326,10.);
#5802=VECTOR('',#21335,10.);
#5803=VECTOR('',#21338,10.);
#5804=VECTOR('',#21339,10.);
#5805=VECTOR('',#21342,10.);
#5806=VECTOR('',#21343,10.);
#5807=VECTOR('',#21344,10.);
#5808=VECTOR('',#21353,10.);
#5809=VECTOR('',#21356,10.);
#5810=VECTOR('',#21357,10.);
#5811=VECTOR('',#21360,10.);
#5812=VECTOR('',#21361,10.);
#5813=VECTOR('',#21362,10.);
#5814=VECTOR('',#21371,10.);
#5815=VECTOR('',#21374,10.);
#5816=VECTOR('',#21375,10.);
#5817=VECTOR('',#21378,10.);
#5818=VECTOR('',#21379,10.);
#5819=VECTOR('',#21380,10.);
#5820=VECTOR('',#21389,10.);
#5821=VECTOR('',#21392,10.);
#5822=VECTOR('',#21393,10.);
#5823=VECTOR('',#21394,10.);
#5824=VECTOR('',#21399,10.);
#5825=VECTOR('',#21406,10.);
#5826=VECTOR('',#21409,10.);
#5827=VECTOR('',#21410,10.);
#5828=VECTOR('',#21411,10.);
#5829=VECTOR('',#21420,10.);
#5830=VECTOR('',#21423,10.);
#5831=VECTOR('',#21424,10.);
#5832=VECTOR('',#21425,10.);
#5833=VECTOR('',#21492,10.);
#5834=VECTOR('',#21493,10.);
#5835=VECTOR('',#21500,10.);
#5836=VECTOR('',#21501,10.);
#5837=VECTOR('',#21502,10.);
#5838=VECTOR('',#21511,10.);
#5839=VECTOR('',#21514,10.);
#5840=VECTOR('',#21515,10.);
#5841=VECTOR('',#21518,10.);
#5842=VECTOR('',#21519,10.);
#5843=VECTOR('',#21520,10.);
#5844=VECTOR('',#21529,10.);
#5845=VECTOR('',#21532,10.);
#5846=VECTOR('',#21533,10.);
#5847=VECTOR('',#21536,10.);
#5848=VECTOR('',#21537,10.);
#5849=VECTOR('',#21538,10.);
#5850=VECTOR('',#21547,10.);
#5851=VECTOR('',#21550,10.);
#5852=VECTOR('',#21551,10.);
#5853=VECTOR('',#21554,10.);
#5854=VECTOR('',#21555,10.);
#5855=VECTOR('',#21556,10.);
#5856=VECTOR('',#21565,10.);
#5857=VECTOR('',#21568,10.);
#5858=VECTOR('',#21569,10.);
#5859=VECTOR('',#21572,10.);
#5860=VECTOR('',#21573,10.);
#5861=VECTOR('',#21574,10.);
#5862=VECTOR('',#21583,10.);
#5863=VECTOR('',#21586,10.);
#5864=VECTOR('',#21587,10.);
#5865=VECTOR('',#21590,10.);
#5866=VECTOR('',#21591,10.);
#5867=VECTOR('',#21592,10.);
#5868=VECTOR('',#21601,10.);
#5869=VECTOR('',#21604,10.);
#5870=VECTOR('',#21605,10.);
#5871=VECTOR('',#21608,10.);
#5872=VECTOR('',#21609,10.);
#5873=VECTOR('',#21610,10.);
#5874=VECTOR('',#21619,10.);
#5875=VECTOR('',#21622,10.);
#5876=VECTOR('',#21623,10.);
#5877=VECTOR('',#21626,10.);
#5878=VECTOR('',#21627,10.);
#5879=VECTOR('',#21628,10.);
#5880=VECTOR('',#21637,10.);
#5881=VECTOR('',#21640,10.);
#5882=VECTOR('',#21641,10.);
#5883=VECTOR('',#21644,10.);
#5884=VECTOR('',#21645,10.);
#5885=VECTOR('',#21646,10.);
#5886=VECTOR('',#21655,10.);
#5887=VECTOR('',#21658,10.);
#5888=VECTOR('',#21659,10.);
#5889=VECTOR('',#21664,10.);
#5890=VECTOR('',#21671,10.);
#5891=VECTOR('',#21740,49.75);
#5892=VECTOR('',#21745,49.5);
#5893=VECTOR('',#21748,10.);
#5894=VECTOR('',#21749,10.);
#5895=VECTOR('',#21820,10.);
#5896=VECTOR('',#21821,10.);
#5897=VECTOR('',#21822,10.);
#5898=VECTOR('',#21829,10.);
#5899=VECTOR('',#21830,10.);
#5900=VECTOR('',#21837,10.);
#5901=VECTOR('',#21838,10.);
#5902=VECTOR('',#21839,10.);
#5903=VECTOR('',#21844,10.);
#5904=VECTOR('',#21847,10.);
#5905=VECTOR('',#21848,10.);
#5906=VECTOR('',#21849,10.);
#5907=VECTOR('',#21856,10.);
#5908=VECTOR('',#21857,10.);
#5909=VECTOR('',#21860,10.);
#5910=VECTOR('',#21865,10.);
#5911=VECTOR('',#21866,10.);
#5912=VECTOR('',#21873,10.);
#5913=VECTOR('',#21874,10.);
#5914=VECTOR('',#21875,10.);
#5915=VECTOR('',#21880,10.);
#5916=VECTOR('',#21883,10.);
#5917=VECTOR('',#21884,10.);
#5918=VECTOR('',#21885,10.);
#5919=VECTOR('',#21892,10.);
#5920=VECTOR('',#21893,10.);
#5921=VECTOR('',#21896,10.);
#5922=VECTOR('',#21901,10.);
#5923=VECTOR('',#21902,10.);
#5924=VECTOR('',#21909,10.);
#5925=VECTOR('',#21910,10.);
#5926=VECTOR('',#21911,10.);
#5927=VECTOR('',#21916,10.);
#5928=VECTOR('',#21919,10.);
#5929=VECTOR('',#21920,10.);
#5930=VECTOR('',#21927,10.);
#5931=VECTOR('',#21928,10.);
#5932=VECTOR('',#21933,52.6267766952966);
#5933=VECTOR('',#21942,53.1);
#5934=VECTOR('',#22149,12.7);
#5935=VECTOR('',#22168,12.5);
#5936=VECTOR('',#22173,12.7);
#5937=VECTOR('',#22178,12.5);
#5938=VECTOR('',#22183,12.7);
#5939=VECTOR('',#22188,12.5);
#5940=VECTOR('',#22193,12.7);
#5941=VECTOR('',#22198,12.5);
#5942=VECTOR('',#22203,12.7);
#5943=VECTOR('',#22208,12.5);
#5944=VECTOR('',#22213,50.8);
#5945=VECTOR('',#22218,50.5);
#5946=VECTOR('',#22447,1.5);
#5947=VECTOR('',#22452,1.5);
#5948=VECTOR('',#22457,1.5);
#5949=VECTOR('',#22462,1.5);
#5950=VECTOR('',#22467,1.5);
#5951=VECTOR('',#22470,5.025);
#5952=VECTOR('',#22479,9.6);
#5953=VECTOR('',#22484,9.6);
#5954=VECTOR('',#22487,9.6);
#5955=VECTOR('',#22490,9.6);
#5956=VECTOR('',#22493,9.6);
#5957=VECTOR('',#22496,9.6);
#5958=VECTOR('',#22499,9.6);
#5959=VECTOR('',#22502,9.6);
#5960=VECTOR('',#22505,9.6);
#5961=VECTOR('',#22508,9.6);
#5962=VECTOR('',#22511,9.6);
#5963=VECTOR('',#22514,9.6);
#5964=VECTOR('',#22519,10.06205);
#5965=VECTOR('',#22524,10.06205);
#5966=VECTOR('',#22527,10.06205);
#5967=VECTOR('',#22530,10.06205);
#5968=VECTOR('',#22533,10.06205);
#5969=VECTOR('',#22536,10.06205);
#5970=VECTOR('',#22539,10.06205);
#5971=VECTOR('',#22542,10.06205);
#5972=VECTOR('',#22545,10.06205);
#5973=VECTOR('',#22548,10.06205);
#5974=VECTOR('',#22551,10.06205);
#5975=VECTOR('',#22554,10.06205);
#5976=VECTOR('',#22569,12.5);
#5977=VECTOR('',#22578,13.5);
#5978=VECTOR('',#22583,13.3);
#5979=VECTOR('',#22590,3.);
#5980=VECTOR('',#22595,3.);
#5981=VECTOR('',#22598,3.);
#5982=VECTOR('',#22601,3.);
#5983=VECTOR('',#22604,3.);
#5984=VECTOR('',#22607,3.);
#5985=VECTOR('',#22610,2.37175);
#5986=VECTOR('',#22615,2.37175);
#5987=VECTOR('',#22618,2.37175);
#5988=VECTOR('',#22621,2.37175);
#5989=VECTOR('',#22624,2.37175);
#5990=VECTOR('',#22627,2.37175);
#5991=VECTOR('',#22650,4.8);
#5992=VECTOR('',#22655,5.);
#5993=VECTOR('',#22662,2.8);
#5994=VECTOR('',#22673,9.56757295257596);
#5995=VECTOR('',#22680,10.3);
#5996=VECTOR('',#22687,7.8);
#5997=VECTOR('',#22696,5.6);
#5998=VECTOR('',#22701,5.);
#5999=VECTOR('',#22710,8.2);
#6000=VECTOR('',#22719,11.);
#6001=VECTOR('',#22730,5.25);
#6002=VECTOR('',#22741,12.);
#6003=VECTOR('',#22750,5.9);
#6004=VECTOR('',#22757,6.);
#6005=VECTOR('',#22766,3.2);
#6006=VECTOR('',#22775,5.9);
#6007=VECTOR('',#22782,3.155);
#6008=VECTOR('',#22787,3.05);
#6009=VECTOR('',#22798,3.155);
#6010=VECTOR('',#22805,4.75273145074145);
#6011=VECTOR('',#22832,10.);
#6012=VECTOR('',#22835,10.);
#6013=VECTOR('',#22838,10.);
#6014=VECTOR('',#22841,10.);
#6015=VECTOR('',#22844,10.);
#6016=VECTOR('',#22847,10.);
#6017=VECTOR('',#22850,10.);
#6018=VECTOR('',#22851,10.);
#6019=VECTOR('',#22854,10.);
#6020=VECTOR('',#22855,10.);
#6021=VECTOR('',#22858,10.);
#6022=VECTOR('',#22859,10.);
#6023=VECTOR('',#22862,10.);
#6024=VECTOR('',#22863,10.);
#6025=VECTOR('',#22866,10.);
#6026=VECTOR('',#22867,10.);
#6027=VECTOR('',#22870,10.);
#6028=VECTOR('',#22871,10.);
#6029=VECTOR('',#22880,5.41175134594813);
#6030=VECTOR('',#22907,2.5);
#6031=VECTOR('',#22912,2.5);
#6032=VECTOR('',#22915,2.5);
#6033=VECTOR('',#22918,2.5);
#6034=VECTOR('',#22921,1.99475);
#6035=VECTOR('',#22926,1.99475);
#6036=VECTOR('',#22929,1.99475);
#6037=VECTOR('',#22932,1.99475);
#6038=VECTOR('',#22951,10.);
#6039=VECTOR('',#22952,10.);
#6040=VECTOR('',#22953,10.);
#6041=VECTOR('',#22954,10.);
#6042=VECTOR('',#22957,10.);
#6043=VECTOR('',#22958,10.);
#6044=VECTOR('',#22959,10.);
#6045=VECTOR('',#22962,10.);
#6046=VECTOR('',#22963,10.);
#6047=VECTOR('',#22964,10.);
#6048=VECTOR('',#22967,10.);
#6049=VECTOR('',#22968,10.);
#6050=VECTOR('',#22969,10.);
#6051=VECTOR('',#22972,10.);
#6052=VECTOR('',#22973,10.);
#6053=VECTOR('',#22974,10.);
#6054=VECTOR('',#22977,10.);
#6055=VECTOR('',#22978,10.);
#6056=VECTOR('',#22987,2.25);
#6057=VECTOR('',#22996,2.35);
#6058=VECTOR('',#23003,2.5);
#6059=VECTOR('',#23008,2.5);
#6060=VECTOR('',#23011,2.5);
#6061=VECTOR('',#23014,2.5);
#6062=VECTOR('',#23017,2.5);
#6063=VECTOR('',#23020,2.5);
#6064=VECTOR('',#23023,2.5);
#6065=VECTOR('',#23026,2.5);
#6066=VECTOR('',#23029,2.5);
#6067=VECTOR('',#23032,2.5);
#6068=VECTOR('',#23035,2.5);
#6069=VECTOR('',#23038,2.5);
#6070=VECTOR('',#23041,2.5);
#6071=VECTOR('',#23044,2.5);
#6072=VECTOR('',#23047,2.5);
#6073=VECTOR('',#23050,1.99475);
#6074=VECTOR('',#23055,1.99475);
#6075=VECTOR('',#23058,1.99475);
#6076=VECTOR('',#23061,1.99475);
#6077=VECTOR('',#23064,1.99475);
#6078=VECTOR('',#23067,1.99475);
#6079=VECTOR('',#23070,1.99475);
#6080=VECTOR('',#23073,1.99475);
#6081=VECTOR('',#23076,1.99475);
#6082=VECTOR('',#23079,1.99475);
#6083=VECTOR('',#23082,1.99475);
#6084=VECTOR('',#23085,1.99475);
#6085=VECTOR('',#23088,1.99475);
#6086=VECTOR('',#23091,1.99475);
#6087=VECTOR('',#23104,10.);
#6088=VECTOR('',#23105,10.);
#6089=VECTOR('',#23106,10.);
#6090=VECTOR('',#23111,10.);
#6091=VECTOR('',#23114,10.);
#6092=VECTOR('',#23119,10.);
#6093=VECTOR('',#23122,10.);
#6094=VECTOR('',#23125,10.);
#6095=VECTOR('',#23128,10.);
#6096=VECTOR('',#23131,10.);
#6097=VECTOR('',#23134,10.);
#6098=VECTOR('',#23137,10.);
#6099=VECTOR('',#23140,10.);
#6100=VECTOR('',#23143,10.);
#6101=VECTOR('',#23146,10.);
#6102=VECTOR('',#23149,10.);
#6103=VECTOR('',#23152,10.);
#6104=VECTOR('',#23155,10.);
#6105=VECTOR('',#23158,10.);
#6106=VECTOR('',#23161,10.);
#6107=VECTOR('',#23164,10.);
#6108=VECTOR('',#23167,10.);
#6109=VECTOR('',#23170,10.);
#6110=VECTOR('',#23173,10.);
#6111=VECTOR('',#23176,10.);
#6112=VECTOR('',#23179,10.);
#6113=VECTOR('',#23182,10.);
#6114=VECTOR('',#23185,10.);
#6115=VECTOR('',#23188,10.);
#6116=VECTOR('',#23191,10.);
#6117=VECTOR('',#23194,10.);
#6118=VECTOR('',#23197,10.);
#6119=VECTOR('',#23200,5.);
#6120=VECTOR('',#23205,10.);
#6121=VECTOR('',#23208,10.);
#6122=VECTOR('',#23211,10.);
#6123=VECTOR('',#23214,10.);
#6124=VECTOR('',#23217,10.);
#6125=VECTOR('',#23220,10.);
#6126=VECTOR('',#23223,10.);
#6127=VECTOR('',#23226,10.);
#6128=VECTOR('',#23229,10.);
#6129=VECTOR('',#23232,10.);
#6130=VECTOR('',#23235,10.);
#6131=VECTOR('',#23238,10.);
#6132=VECTOR('',#23241,10.);
#6133=VECTOR('',#23244,10.);
#6134=VECTOR('',#23247,10.);
#6135=VECTOR('',#23250,10.);
#6136=VECTOR('',#23253,10.);
#6137=VECTOR('',#23256,10.);
#6138=VECTOR('',#23259,10.);
#6139=VECTOR('',#23262,10.);
#6140=VECTOR('',#23265,10.);
#6141=VECTOR('',#23268,10.);
#6142=VECTOR('',#23271,10.);
#6143=VECTOR('',#23274,10.);
#6144=VECTOR('',#23277,10.);
#6145=VECTOR('',#23280,10.);
#6146=VECTOR('',#23283,10.);
#6147=VECTOR('',#23286,10.);
#6148=VECTOR('',#23289,10.);
#6149=VECTOR('',#23292,10.);
#6150=VECTOR('',#23295,10.);
#6151=VECTOR('',#23300,10.);
#6152=VECTOR('',#23301,10.);
#6153=VECTOR('',#23304,10.);
#6154=VECTOR('',#23309,10.);
#6155=VECTOR('',#23310,10.);
#6156=VECTOR('',#23313,10.);
#6157=VECTOR('',#23318,10.);
#6158=VECTOR('',#23319,10.);
#6159=VECTOR('',#23322,10.);
#6160=VECTOR('',#23327,10.);
#6161=VECTOR('',#23328,10.);
#6162=VECTOR('',#23331,10.);
#6163=VECTOR('',#23336,10.);
#6164=VECTOR('',#23337,10.);
#6165=VECTOR('',#23340,10.);
#6166=VECTOR('',#23345,10.);
#6167=VECTOR('',#23346,10.);
#6168=VECTOR('',#23349,10.);
#6169=VECTOR('',#23354,10.);
#6170=VECTOR('',#23355,10.);
#6171=VECTOR('',#23358,10.);
#6172=VECTOR('',#23363,10.);
#6173=VECTOR('',#23364,10.);
#6174=VECTOR('',#23367,10.);
#6175=VECTOR('',#23372,10.);
#6176=VECTOR('',#23373,10.);
#6177=VECTOR('',#23376,10.);
#6178=VECTOR('',#23381,10.);
#6179=VECTOR('',#23382,10.);
#6180=VECTOR('',#23385,10.);
#6181=VECTOR('',#23390,10.);
#6182=VECTOR('',#23391,10.);
#6183=VECTOR('',#23394,10.);
#6184=VECTOR('',#23399,10.);
#6185=VECTOR('',#23400,10.);
#6186=VECTOR('',#23403,10.);
#6187=VECTOR('',#23408,10.);
#6188=VECTOR('',#23409,10.);
#6189=VECTOR('',#23412,10.);
#6190=VECTOR('',#23417,10.);
#6191=VECTOR('',#23418,10.);
#6192=VECTOR('',#23421,10.);
#6193=VECTOR('',#23426,10.);
#6194=VECTOR('',#23427,10.);
#6195=VECTOR('',#23430,10.);
#6196=VECTOR('',#23435,10.);
#6197=VECTOR('',#23436,10.);
#6198=VECTOR('',#23439,10.);
#6199=VECTOR('',#23444,10.);
#6200=VECTOR('',#23445,10.);
#6201=VECTOR('',#23448,10.);
#6202=VECTOR('',#23453,10.);
#6203=VECTOR('',#23454,10.);
#6204=VECTOR('',#23457,10.);
#6205=VECTOR('',#23462,10.);
#6206=VECTOR('',#23463,10.);
#6207=VECTOR('',#23466,10.);
#6208=VECTOR('',#23471,10.);
#6209=VECTOR('',#23472,10.);
#6210=VECTOR('',#23475,10.);
#6211=VECTOR('',#23480,10.);
#6212=VECTOR('',#23481,10.);
#6213=VECTOR('',#23484,10.);
#6214=VECTOR('',#23489,10.);
#6215=VECTOR('',#23490,10.);
#6216=VECTOR('',#23493,10.);
#6217=VECTOR('',#23498,10.);
#6218=VECTOR('',#23499,10.);
#6219=VECTOR('',#23502,10.);
#6220=VECTOR('',#23507,10.);
#6221=VECTOR('',#23508,10.);
#6222=VECTOR('',#23511,10.);
#6223=VECTOR('',#23516,10.);
#6224=VECTOR('',#23517,10.);
#6225=VECTOR('',#23520,10.);
#6226=VECTOR('',#23525,10.);
#6227=VECTOR('',#23526,10.);
#6228=VECTOR('',#23529,10.);
#6229=VECTOR('',#23534,10.);
#6230=VECTOR('',#23535,10.);
#6231=VECTOR('',#23538,10.);
#6232=VECTOR('',#23543,10.);
#6233=VECTOR('',#23544,10.);
#6234=VECTOR('',#23547,10.);
#6235=VECTOR('',#23552,10.);
#6236=VECTOR('',#23553,10.);
#6237=VECTOR('',#23556,10.);
#6238=VECTOR('',#23565,2.3);
#6239=VECTOR('',#23576,4.75);
#6240=VECTOR('',#23581,4.7);
#6241=VERTEX_POINT('',#23619);
#6242=VERTEX_POINT('',#23620);
#6243=VERTEX_POINT('',#23622);
#6244=VERTEX_POINT('',#23624);
#6245=VERTEX_POINT('',#23628);
#6246=VERTEX_POINT('',#23629);
#6247=VERTEX_POINT('',#23631);
#6248=VERTEX_POINT('',#23633);
#6249=VERTEX_POINT('',#23643);
#6250=VERTEX_POINT('',#23645);
#6251=VERTEX_POINT('',#23649);
#6252=VERTEX_POINT('',#23653);
#6253=VERTEX_POINT('',#23654);
#6254=VERTEX_POINT('',#23656);
#6255=VERTEX_POINT('',#23658);
#6256=VERTEX_POINT('',#23660);
#6257=VERTEX_POINT('',#23663);
#6258=VERTEX_POINT('',#23664);
#6259=VERTEX_POINT('',#23666);
#6260=VERTEX_POINT('',#23668);
#6261=VERTEX_POINT('',#23671);
#6262=VERTEX_POINT('',#23672);
#6263=VERTEX_POINT('',#23674);
#6264=VERTEX_POINT('',#23676);
#6265=VERTEX_POINT('',#23679);
#6266=VERTEX_POINT('',#23680);
#6267=VERTEX_POINT('',#23682);
#6268=VERTEX_POINT('',#23684);
#6269=VERTEX_POINT('',#23688);
#6270=VERTEX_POINT('',#23689);
#6271=VERTEX_POINT('',#23694);
#6272=VERTEX_POINT('',#23698);
#6273=VERTEX_POINT('',#23702);
#6274=VERTEX_POINT('',#23704);
#6275=VERTEX_POINT('',#23708);
#6276=VERTEX_POINT('',#23712);
#6277=VERTEX_POINT('',#23716);
#6278=VERTEX_POINT('',#23718);
#6279=VERTEX_POINT('',#23722);
#6280=VERTEX_POINT('',#23724);
#6281=VERTEX_POINT('',#23728);
#6282=VERTEX_POINT('',#23730);
#6283=VERTEX_POINT('',#23734);
#6284=VERTEX_POINT('',#23736);
#6285=VERTEX_POINT('',#23740);
#6286=VERTEX_POINT('',#23742);
#6287=VERTEX_POINT('',#23746);
#6288=VERTEX_POINT('',#23748);
#6289=VERTEX_POINT('',#23752);
#6290=VERTEX_POINT('',#23754);
#6291=VERTEX_POINT('',#23758);
#6292=VERTEX_POINT('',#23760);
#6293=VERTEX_POINT('',#23764);
#6294=VERTEX_POINT('',#23765);
#6295=VERTEX_POINT('',#23770);
#6296=VERTEX_POINT('',#23774);
#6297=VERTEX_POINT('',#23776);
#6298=VERTEX_POINT('',#23780);
#6299=VERTEX_POINT('',#23784);
#6300=VERTEX_POINT('',#23785);
#6301=VERTEX_POINT('',#23788);
#6302=VERTEX_POINT('',#23794);
#6303=VERTEX_POINT('',#23795);
#6304=VERTEX_POINT('',#23798);
#6305=VERTEX_POINT('',#23802);
#6306=VERTEX_POINT('',#23804);
#6307=VERTEX_POINT('',#23810);
#6308=VERTEX_POINT('',#23812);
#6309=VERTEX_POINT('',#23816);
#6310=VERTEX_POINT('',#23817);
#6311=VERTEX_POINT('',#23827);
#6312=VERTEX_POINT('',#23829);
#6313=VERTEX_POINT('',#23831);
#6314=VERTEX_POINT('',#23833);
#6315=VERTEX_POINT('',#23835);
#6316=VERTEX_POINT('',#23837);
#6317=VERTEX_POINT('',#23876);
#6318=VERTEX_POINT('',#23878);
#6319=VERTEX_POINT('',#23882);
#6320=VERTEX_POINT('',#23884);
#6321=VERTEX_POINT('',#23887);
#6322=VERTEX_POINT('',#23888);
#6323=VERTEX_POINT('',#23915);
#6324=VERTEX_POINT('',#23919);
#6325=VERTEX_POINT('',#23933);
#6326=VERTEX_POINT('',#23936);
#6327=VERTEX_POINT('',#23938);
#6328=VERTEX_POINT('',#23942);
#6329=VERTEX_POINT('',#23948);
#6330=VERTEX_POINT('',#23952);
#6331=VERTEX_POINT('',#23956);
#6332=VERTEX_POINT('',#23960);
#6333=VERTEX_POINT('',#23962);
#6334=VERTEX_POINT('',#23964);
#6335=VERTEX_POINT('',#23969);
#6336=VERTEX_POINT('',#23974);
#6337=VERTEX_POINT('',#23979);
#6338=VERTEX_POINT('',#23987);
#6339=VERTEX_POINT('',#23995);
#6340=VERTEX_POINT('',#23996);
#6341=VERTEX_POINT('',#24000);
#6342=VERTEX_POINT('',#24002);
#6343=VERTEX_POINT('',#24006);
#6344=VERTEX_POINT('',#24008);
#6345=VERTEX_POINT('',#24012);
#6346=VERTEX_POINT('',#24017);
#6347=VERTEX_POINT('',#24019);
#6348=VERTEX_POINT('',#24028);
#6349=VERTEX_POINT('',#24029);
#6350=VERTEX_POINT('',#24033);
#6351=VERTEX_POINT('',#24035);
#6352=VERTEX_POINT('',#24037);
#6353=VERTEX_POINT('',#24043);
#6354=VERTEX_POINT('',#24045);
#6355=VERTEX_POINT('',#24049);
#6356=VERTEX_POINT('',#24054);
#6357=VERTEX_POINT('',#24056);
#6358=VERTEX_POINT('',#24065);
#6359=VERTEX_POINT('',#24069);
#6360=VERTEX_POINT('',#24071);
#6361=VERTEX_POINT('',#24076);
#6362=VERTEX_POINT('',#24080);
#6363=VERTEX_POINT('',#24081);
#6364=VERTEX_POINT('',#24085);
#6365=VERTEX_POINT('',#24087);
#6366=VERTEX_POINT('',#24089);
#6367=VERTEX_POINT('',#24095);
#6368=VERTEX_POINT('',#24097);
#6369=VERTEX_POINT('',#24101);
#6370=VERTEX_POINT('',#24106);
#6371=VERTEX_POINT('',#24113);
#6372=VERTEX_POINT('',#24117);
#6373=VERTEX_POINT('',#24118);
#6374=VERTEX_POINT('',#24120);
#6375=VERTEX_POINT('',#24122);
#6376=VERTEX_POINT('',#24126);
#6377=VERTEX_POINT('',#24135);
#6378=VERTEX_POINT('',#24142);
#6379=VERTEX_POINT('',#24143);
#6380=VERTEX_POINT('',#24147);
#6381=VERTEX_POINT('',#24149);
#6382=VERTEX_POINT('',#24151);
#6383=VERTEX_POINT('',#24157);
#6384=VERTEX_POINT('',#24159);
#6385=VERTEX_POINT('',#24163);
#6386=VERTEX_POINT('',#24168);
#6387=VERTEX_POINT('',#24175);
#6388=VERTEX_POINT('',#24179);
#6389=VERTEX_POINT('',#24181);
#6390=VERTEX_POINT('',#24187);
#6391=VERTEX_POINT('',#24189);
#6392=VERTEX_POINT('',#24195);
#6393=VERTEX_POINT('',#24196);
#6394=VERTEX_POINT('',#24198);
#6395=VERTEX_POINT('',#24200);
#6396=VERTEX_POINT('',#24206);
#6397=VERTEX_POINT('',#24211);
#6398=VERTEX_POINT('',#24213);
#6399=VERTEX_POINT('',#24218);
#6400=VERTEX_POINT('',#24222);
#6401=VERTEX_POINT('',#24224);
#6402=VERTEX_POINT('',#24229);
#6403=VERTEX_POINT('',#24236);
#6404=VERTEX_POINT('',#24237);
#6405=VERTEX_POINT('',#24241);
#6406=VERTEX_POINT('',#24243);
#6407=VERTEX_POINT('',#24245);
#6408=VERTEX_POINT('',#24251);
#6409=VERTEX_POINT('',#24253);
#6410=VERTEX_POINT('',#24257);
#6411=VERTEX_POINT('',#24262);
#6412=VERTEX_POINT('',#24264);
#6413=VERTEX_POINT('',#24274);
#6414=VERTEX_POINT('',#24275);
#6415=VERTEX_POINT('',#24277);
#6416=VERTEX_POINT('',#24279);
#6417=VERTEX_POINT('',#24283);
#6418=VERTEX_POINT('',#24289);
#6419=VERTEX_POINT('',#24291);
#6420=VERTEX_POINT('',#24295);
#6421=VERTEX_POINT('',#24300);
#6422=VERTEX_POINT('',#24307);
#6423=VERTEX_POINT('',#24311);
#6424=VERTEX_POINT('',#24313);
#6425=VERTEX_POINT('',#24319);
#6426=VERTEX_POINT('',#24320);
#6427=VERTEX_POINT('',#24322);
#6428=VERTEX_POINT('',#24324);
#6429=VERTEX_POINT('',#24328);
#6430=VERTEX_POINT('',#24334);
#6431=VERTEX_POINT('',#24336);
#6432=VERTEX_POINT('',#24340);
#6433=VERTEX_POINT('',#24345);
#6434=VERTEX_POINT('',#24352);
#6435=VERTEX_POINT('',#24356);
#6436=VERTEX_POINT('',#24358);
#6437=VERTEX_POINT('',#24364);
#6438=VERTEX_POINT('',#24365);
#6439=VERTEX_POINT('',#24367);
#6440=VERTEX_POINT('',#24369);
#6441=VERTEX_POINT('',#24373);
#6442=VERTEX_POINT('',#24379);
#6443=VERTEX_POINT('',#24381);
#6444=VERTEX_POINT('',#24385);
#6445=VERTEX_POINT('',#24390);
#6446=VERTEX_POINT('',#24397);
#6447=VERTEX_POINT('',#24401);
#6448=VERTEX_POINT('',#24403);
#6449=VERTEX_POINT('',#24409);
#6450=VERTEX_POINT('',#24410);
#6451=VERTEX_POINT('',#24412);
#6452=VERTEX_POINT('',#24414);
#6453=VERTEX_POINT('',#24418);
#6454=VERTEX_POINT('',#24424);
#6455=VERTEX_POINT('',#24426);
#6456=VERTEX_POINT('',#24430);
#6457=VERTEX_POINT('',#24435);
#6458=VERTEX_POINT('',#24442);
#6459=VERTEX_POINT('',#24446);
#6460=VERTEX_POINT('',#24448);
#6461=VERTEX_POINT('',#24454);
#6462=VERTEX_POINT('',#24455);
#6463=VERTEX_POINT('',#24457);
#6464=VERTEX_POINT('',#24459);
#6465=VERTEX_POINT('',#24463);
#6466=VERTEX_POINT('',#24469);
#6467=VERTEX_POINT('',#24471);
#6468=VERTEX_POINT('',#24475);
#6469=VERTEX_POINT('',#24480);
#6470=VERTEX_POINT('',#24487);
#6471=VERTEX_POINT('',#24491);
#6472=VERTEX_POINT('',#24493);
#6473=VERTEX_POINT('',#24499);
#6474=VERTEX_POINT('',#24500);
#6475=VERTEX_POINT('',#24502);
#6476=VERTEX_POINT('',#24504);
#6477=VERTEX_POINT('',#24508);
#6478=VERTEX_POINT('',#24514);
#6479=VERTEX_POINT('',#24516);
#6480=VERTEX_POINT('',#24520);
#6481=VERTEX_POINT('',#24525);
#6482=VERTEX_POINT('',#24532);
#6483=VERTEX_POINT('',#24536);
#6484=VERTEX_POINT('',#24538);
#6485=VERTEX_POINT('',#24544);
#6486=VERTEX_POINT('',#24545);
#6487=VERTEX_POINT('',#24547);
#6488=VERTEX_POINT('',#24549);
#6489=VERTEX_POINT('',#24553);
#6490=VERTEX_POINT('',#24559);
#6491=VERTEX_POINT('',#24561);
#6492=VERTEX_POINT('',#24565);
#6493=VERTEX_POINT('',#24570);
#6494=VERTEX_POINT('',#24577);
#6495=VERTEX_POINT('',#24581);
#6496=VERTEX_POINT('',#24583);
#6497=VERTEX_POINT('',#24589);
#6498=VERTEX_POINT('',#24590);
#6499=VERTEX_POINT('',#24592);
#6500=VERTEX_POINT('',#24594);
#6501=VERTEX_POINT('',#24598);
#6502=VERTEX_POINT('',#24604);
#6503=VERTEX_POINT('',#24606);
#6504=VERTEX_POINT('',#24610);
#6505=VERTEX_POINT('',#24615);
#6506=VERTEX_POINT('',#24622);
#6507=VERTEX_POINT('',#24626);
#6508=VERTEX_POINT('',#24628);
#6509=VERTEX_POINT('',#24634);
#6510=VERTEX_POINT('',#24636);
#6511=VERTEX_POINT('',#24640);
#6512=VERTEX_POINT('',#24655);
#6513=VERTEX_POINT('',#24657);
#6514=VERTEX_POINT('',#24661);
#6515=VERTEX_POINT('',#24668);
#6516=VERTEX_POINT('',#24670);
#6517=VERTEX_POINT('',#24672);
#6518=VERTEX_POINT('',#24674);
#6519=VERTEX_POINT('',#24676);
#6520=VERTEX_POINT('',#24678);
#6521=VERTEX_POINT('',#24680);
#6522=VERTEX_POINT('',#24682);
#6523=VERTEX_POINT('',#24684);
#6524=VERTEX_POINT('',#24686);
#6525=VERTEX_POINT('',#24688);
#6526=VERTEX_POINT('',#24700);
#6527=VERTEX_POINT('',#24702);
#6528=VERTEX_POINT('',#24704);
#6529=VERTEX_POINT('',#24706);
#6530=VERTEX_POINT('',#24708);
#6531=VERTEX_POINT('',#24710);
#6532=VERTEX_POINT('',#24712);
#6533=VERTEX_POINT('',#24714);
#6534=VERTEX_POINT('',#24716);
#6535=VERTEX_POINT('',#24718);
#6536=VERTEX_POINT('',#24720);
#6537=VERTEX_POINT('',#24722);
#6538=VERTEX_POINT('',#24724);
#6539=VERTEX_POINT('',#24726);
#6540=VERTEX_POINT('',#24728);
#6541=VERTEX_POINT('',#24730);
#6542=VERTEX_POINT('',#24732);
#6543=VERTEX_POINT('',#24735);
#6544=VERTEX_POINT('',#24737);
#6545=VERTEX_POINT('',#24739);
#6546=VERTEX_POINT('',#24741);
#6547=VERTEX_POINT('',#24743);
#6548=VERTEX_POINT('',#24745);
#6549=VERTEX_POINT('',#24747);
#6550=VERTEX_POINT('',#24749);
#6551=VERTEX_POINT('',#24751);
#6552=VERTEX_POINT('',#24753);
#6553=VERTEX_POINT('',#24755);
#6554=VERTEX_POINT('',#24757);
#6555=VERTEX_POINT('',#24759);
#6556=VERTEX_POINT('',#24761);
#6557=VERTEX_POINT('',#24763);
#6558=VERTEX_POINT('',#24765);
#6559=VERTEX_POINT('',#24767);
#6560=VERTEX_POINT('',#24769);
#6561=VERTEX_POINT('',#24771);
#6562=VERTEX_POINT('',#24773);
#6563=VERTEX_POINT('',#24775);
#6564=VERTEX_POINT('',#24777);
#6565=VERTEX_POINT('',#24779);
#6566=VERTEX_POINT('',#24781);
#6567=VERTEX_POINT('',#24783);
#6568=VERTEX_POINT('',#24785);
#6569=VERTEX_POINT('',#24787);
#6570=VERTEX_POINT('',#24789);
#6571=VERTEX_POINT('',#24791);
#6572=VERTEX_POINT('',#24793);
#6573=VERTEX_POINT('',#24795);
#6574=VERTEX_POINT('',#24797);
#6575=VERTEX_POINT('',#24799);
#6576=VERTEX_POINT('',#24801);
#6577=VERTEX_POINT('',#24803);
#6578=VERTEX_POINT('',#24805);
#6579=VERTEX_POINT('',#24807);
#6580=VERTEX_POINT('',#24809);
#6581=VERTEX_POINT('',#24811);
#6582=VERTEX_POINT('',#24813);
#6583=VERTEX_POINT('',#24815);
#6584=VERTEX_POINT('',#24817);
#6585=VERTEX_POINT('',#24819);
#6586=VERTEX_POINT('',#24821);
#6587=VERTEX_POINT('',#24823);
#6588=VERTEX_POINT('',#24825);
#6589=VERTEX_POINT('',#24827);
#6590=VERTEX_POINT('',#24829);
#6591=VERTEX_POINT('',#24831);
#6592=VERTEX_POINT('',#24833);
#6593=VERTEX_POINT('',#24835);
#6594=VERTEX_POINT('',#24837);
#6595=VERTEX_POINT('',#24839);
#6596=VERTEX_POINT('',#24841);
#6597=VERTEX_POINT('',#24843);
#6598=VERTEX_POINT('',#24845);
#6599=VERTEX_POINT('',#24847);
#6600=VERTEX_POINT('',#24849);
#6601=VERTEX_POINT('',#24851);
#6602=VERTEX_POINT('',#24853);
#6603=VERTEX_POINT('',#24855);
#6604=VERTEX_POINT('',#24857);
#6605=VERTEX_POINT('',#24859);
#6606=VERTEX_POINT('',#24861);
#6607=VERTEX_POINT('',#24863);
#6608=VERTEX_POINT('',#24865);
#6609=VERTEX_POINT('',#24867);
#6610=VERTEX_POINT('',#24869);
#6611=VERTEX_POINT('',#24871);
#6612=VERTEX_POINT('',#24873);
#6613=VERTEX_POINT('',#24875);
#6614=VERTEX_POINT('',#24877);
#6615=VERTEX_POINT('',#24879);
#6616=VERTEX_POINT('',#24881);
#6617=VERTEX_POINT('',#24883);
#6618=VERTEX_POINT('',#24885);
#6619=VERTEX_POINT('',#24887);
#6620=VERTEX_POINT('',#24889);
#6621=VERTEX_POINT('',#24891);
#6622=VERTEX_POINT('',#24893);
#6623=VERTEX_POINT('',#24895);
#6624=VERTEX_POINT('',#24897);
#6625=VERTEX_POINT('',#24899);
#6626=VERTEX_POINT('',#24901);
#6627=VERTEX_POINT('',#24903);
#6628=VERTEX_POINT('',#24905);
#6629=VERTEX_POINT('',#24907);
#6630=VERTEX_POINT('',#24909);
#6631=VERTEX_POINT('',#24911);
#6632=VERTEX_POINT('',#24913);
#6633=VERTEX_POINT('',#24915);
#6634=VERTEX_POINT('',#24917);
#6635=VERTEX_POINT('',#24919);
#6636=VERTEX_POINT('',#24921);
#6637=VERTEX_POINT('',#24923);
#6638=VERTEX_POINT('',#24925);
#6639=VERTEX_POINT('',#24927);
#6640=VERTEX_POINT('',#24929);
#6641=VERTEX_POINT('',#24931);
#6642=VERTEX_POINT('',#24933);
#6643=VERTEX_POINT('',#24935);
#6644=VERTEX_POINT('',#24937);
#6645=VERTEX_POINT('',#24939);
#6646=VERTEX_POINT('',#24941);
#6647=VERTEX_POINT('',#24943);
#6648=VERTEX_POINT('',#24945);
#6649=VERTEX_POINT('',#24947);
#6650=VERTEX_POINT('',#24949);
#6651=VERTEX_POINT('',#24951);
#6652=VERTEX_POINT('',#24953);
#6653=VERTEX_POINT('',#24955);
#6654=VERTEX_POINT('',#24957);
#6655=VERTEX_POINT('',#24959);
#6656=VERTEX_POINT('',#24961);
#6657=VERTEX_POINT('',#24963);
#6658=VERTEX_POINT('',#24965);
#6659=VERTEX_POINT('',#24967);
#6660=VERTEX_POINT('',#24969);
#6661=VERTEX_POINT('',#24971);
#6662=VERTEX_POINT('',#24974);
#6663=VERTEX_POINT('',#24977);
#6664=VERTEX_POINT('',#24979);
#6665=VERTEX_POINT('',#24981);
#6666=VERTEX_POINT('',#24988);
#6667=VERTEX_POINT('',#24992);
#6668=VERTEX_POINT('',#24993);
#6669=VERTEX_POINT('',#24997);
#6670=VERTEX_POINT('',#24999);
#6671=VERTEX_POINT('',#25001);
#6672=VERTEX_POINT('',#25007);
#6673=VERTEX_POINT('',#25009);
#6674=VERTEX_POINT('',#25022);
#6675=VERTEX_POINT('',#25026);
#6676=VERTEX_POINT('',#25028);
#6677=VERTEX_POINT('',#25034);
#6678=VERTEX_POINT('',#25035);
#6679=VERTEX_POINT('',#25039);
#6680=VERTEX_POINT('',#25041);
#6681=VERTEX_POINT('',#25043);
#6682=VERTEX_POINT('',#25049);
#6683=VERTEX_POINT('',#25051);
#6684=VERTEX_POINT('',#25064);
#6685=VERTEX_POINT('',#25068);
#6686=VERTEX_POINT('',#25070);
#6687=VERTEX_POINT('',#25076);
#6688=VERTEX_POINT('',#25077);
#6689=VERTEX_POINT('',#25081);
#6690=VERTEX_POINT('',#25083);
#6691=VERTEX_POINT('',#25085);
#6692=VERTEX_POINT('',#25091);
#6693=VERTEX_POINT('',#25093);
#6694=VERTEX_POINT('',#25106);
#6695=VERTEX_POINT('',#25110);
#6696=VERTEX_POINT('',#25114);
#6697=VERTEX_POINT('',#25118);
#6698=VERTEX_POINT('',#25120);
#6699=VERTEX_POINT('',#25130);
#6700=VERTEX_POINT('',#25131);
#6701=VERTEX_POINT('',#25133);
#6702=VERTEX_POINT('',#25135);
#6703=VERTEX_POINT('',#25141);
#6704=VERTEX_POINT('',#25143);
#6705=VERTEX_POINT('',#25156);
#6706=VERTEX_POINT('',#25160);
#6707=VERTEX_POINT('',#25162);
#6708=VERTEX_POINT('',#25168);
#6709=VERTEX_POINT('',#25169);
#6710=VERTEX_POINT('',#25171);
#6711=VERTEX_POINT('',#25173);
#6712=VERTEX_POINT('',#25177);
#6713=VERTEX_POINT('',#25183);
#6714=VERTEX_POINT('',#25185);
#6715=VERTEX_POINT('',#25198);
#6716=VERTEX_POINT('',#25202);
#6717=VERTEX_POINT('',#25204);
#6718=VERTEX_POINT('',#25210);
#6719=VERTEX_POINT('',#25211);
#6720=VERTEX_POINT('',#25213);
#6721=VERTEX_POINT('',#25215);
#6722=VERTEX_POINT('',#25219);
#6723=VERTEX_POINT('',#25225);
#6724=VERTEX_POINT('',#25227);
#6725=VERTEX_POINT('',#25240);
#6726=VERTEX_POINT('',#25244);
#6727=VERTEX_POINT('',#25246);
#6728=VERTEX_POINT('',#25252);
#6729=VERTEX_POINT('',#25253);
#6730=VERTEX_POINT('',#25255);
#6731=VERTEX_POINT('',#25257);
#6732=VERTEX_POINT('',#25261);
#6733=VERTEX_POINT('',#25267);
#6734=VERTEX_POINT('',#25269);
#6735=VERTEX_POINT('',#25282);
#6736=VERTEX_POINT('',#25286);
#6737=VERTEX_POINT('',#25288);
#6738=VERTEX_POINT('',#25294);
#6739=VERTEX_POINT('',#25295);
#6740=VERTEX_POINT('',#25297);
#6741=VERTEX_POINT('',#25299);
#6742=VERTEX_POINT('',#25303);
#6743=VERTEX_POINT('',#25309);
#6744=VERTEX_POINT('',#25311);
#6745=VERTEX_POINT('',#25324);
#6746=VERTEX_POINT('',#25328);
#6747=VERTEX_POINT('',#25330);
#6748=VERTEX_POINT('',#25336);
#6749=VERTEX_POINT('',#25337);
#6750=VERTEX_POINT('',#25339);
#6751=VERTEX_POINT('',#25341);
#6752=VERTEX_POINT('',#25345);
#6753=VERTEX_POINT('',#25351);
#6754=VERTEX_POINT('',#25353);
#6755=VERTEX_POINT('',#25366);
#6756=VERTEX_POINT('',#25370);
#6757=VERTEX_POINT('',#25371);
#6758=VERTEX_POINT('',#25373);
#6759=VERTEX_POINT('',#25375);
#6760=VERTEX_POINT('',#25398);
#6761=VERTEX_POINT('',#25424);
#6762=VERTEX_POINT('',#25425);
#6763=VERTEX_POINT('',#25429);
#6764=VERTEX_POINT('',#25431);
#6765=VERTEX_POINT('',#25433);
#6766=VERTEX_POINT('',#25439);
#6767=VERTEX_POINT('',#25441);
#6768=VERTEX_POINT('',#25454);
#6769=VERTEX_POINT('',#25458);
#6770=VERTEX_POINT('',#25460);
#6771=VERTEX_POINT('',#25466);
#6772=VERTEX_POINT('',#25468);
#6773=VERTEX_POINT('',#25477);
#6774=VERTEX_POINT('',#25479);
#6775=VERTEX_POINT('',#25481);
#6776=VERTEX_POINT('',#25487);
#6777=VERTEX_POINT('',#25489);
#6778=VERTEX_POINT('',#25498);
#6779=VERTEX_POINT('',#25502);
#6780=VERTEX_POINT('',#25504);
#6781=VERTEX_POINT('',#25510);
#6782=VERTEX_POINT('',#25511);
#6783=VERTEX_POINT('',#25515);
#6784=VERTEX_POINT('',#25517);
#6785=VERTEX_POINT('',#25519);
#6786=VERTEX_POINT('',#25525);
#6787=VERTEX_POINT('',#25527);
#6788=VERTEX_POINT('',#25540);
#6789=VERTEX_POINT('',#25544);
#6790=VERTEX_POINT('',#25546);
#6791=VERTEX_POINT('',#25552);
#6792=VERTEX_POINT('',#25553);
#6793=VERTEX_POINT('',#25557);
#6794=VERTEX_POINT('',#25559);
#6795=VERTEX_POINT('',#25561);
#6796=VERTEX_POINT('',#25567);
#6797=VERTEX_POINT('',#25569);
#6798=VERTEX_POINT('',#25582);
#6799=VERTEX_POINT('',#25586);
#6800=VERTEX_POINT('',#25587);
#6801=VERTEX_POINT('',#25591);
#6802=VERTEX_POINT('',#25593);
#6803=VERTEX_POINT('',#25597);
#6804=VERTEX_POINT('',#25599);
#6805=VERTEX_POINT('',#25613);
#6806=VERTEX_POINT('',#25614);
#6807=VERTEX_POINT('',#25616);
#6808=VERTEX_POINT('',#25618);
#6809=VERTEX_POINT('',#25624);
#6810=VERTEX_POINT('',#25626);
#6811=VERTEX_POINT('',#25639);
#6812=VERTEX_POINT('',#25643);
#6813=VERTEX_POINT('',#25645);
#6814=VERTEX_POINT('',#25651);
#6815=VERTEX_POINT('',#25652);
#6816=VERTEX_POINT('',#25654);
#6817=VERTEX_POINT('',#25656);
#6818=VERTEX_POINT('',#25660);
#6819=VERTEX_POINT('',#25666);
#6820=VERTEX_POINT('',#25668);
#6821=VERTEX_POINT('',#25681);
#6822=VERTEX_POINT('',#25685);
#6823=VERTEX_POINT('',#25687);
#6824=VERTEX_POINT('',#25693);
#6825=VERTEX_POINT('',#25694);
#6826=VERTEX_POINT('',#25696);
#6827=VERTEX_POINT('',#25698);
#6828=VERTEX_POINT('',#25702);
#6829=VERTEX_POINT('',#25708);
#6830=VERTEX_POINT('',#25710);
#6831=VERTEX_POINT('',#25723);
#6832=VERTEX_POINT('',#25727);
#6833=VERTEX_POINT('',#25729);
#6834=VERTEX_POINT('',#25735);
#6835=VERTEX_POINT('',#25736);
#6836=VERTEX_POINT('',#25738);
#6837=VERTEX_POINT('',#25740);
#6838=VERTEX_POINT('',#25744);
#6839=VERTEX_POINT('',#25750);
#6840=VERTEX_POINT('',#25752);
#6841=VERTEX_POINT('',#25765);
#6842=VERTEX_POINT('',#25769);
#6843=VERTEX_POINT('',#25771);
#6844=VERTEX_POINT('',#25777);
#6845=VERTEX_POINT('',#25778);
#6846=VERTEX_POINT('',#25780);
#6847=VERTEX_POINT('',#25782);
#6848=VERTEX_POINT('',#25786);
#6849=VERTEX_POINT('',#25792);
#6850=VERTEX_POINT('',#25794);
#6851=VERTEX_POINT('',#25807);
#6852=VERTEX_POINT('',#25811);
#6853=VERTEX_POINT('',#25812);
#6854=VERTEX_POINT('',#25814);
#6855=VERTEX_POINT('',#25816);
#6856=VERTEX_POINT('',#25841);
#6857=VERTEX_POINT('',#25863);
#6858=VERTEX_POINT('',#25864);
#6859=VERTEX_POINT('',#25868);
#6860=VERTEX_POINT('',#25870);
#6861=VERTEX_POINT('',#25872);
#6862=VERTEX_POINT('',#25878);
#6863=VERTEX_POINT('',#25880);
#6864=VERTEX_POINT('',#25893);
#6865=VERTEX_POINT('',#25897);
#6866=VERTEX_POINT('',#25899);
#6867=VERTEX_POINT('',#25905);
#6868=VERTEX_POINT('',#25906);
#6869=VERTEX_POINT('',#25910);
#6870=VERTEX_POINT('',#25912);
#6871=VERTEX_POINT('',#25914);
#6872=VERTEX_POINT('',#25920);
#6873=VERTEX_POINT('',#25922);
#6874=VERTEX_POINT('',#25935);
#6875=VERTEX_POINT('',#25939);
#6876=VERTEX_POINT('',#25941);
#6877=VERTEX_POINT('',#25947);
#6878=VERTEX_POINT('',#25948);
#6879=VERTEX_POINT('',#25952);
#6880=VERTEX_POINT('',#25954);
#6881=VERTEX_POINT('',#25956);
#6882=VERTEX_POINT('',#25962);
#6883=VERTEX_POINT('',#25964);
#6884=VERTEX_POINT('',#25977);
#6885=VERTEX_POINT('',#25981);
#6886=VERTEX_POINT('',#25983);
#6887=VERTEX_POINT('',#25989);
#6888=VERTEX_POINT('',#25990);
#6889=VERTEX_POINT('',#25994);
#6890=VERTEX_POINT('',#25996);
#6891=VERTEX_POINT('',#25998);
#6892=VERTEX_POINT('',#26004);
#6893=VERTEX_POINT('',#26006);
#6894=VERTEX_POINT('',#26019);
#6895=VERTEX_POINT('',#26023);
#6896=VERTEX_POINT('',#26025);
#6897=VERTEX_POINT('',#26031);
#6898=VERTEX_POINT('',#26032);
#6899=VERTEX_POINT('',#26036);
#6900=VERTEX_POINT('',#26038);
#6901=VERTEX_POINT('',#26040);
#6902=VERTEX_POINT('',#26046);
#6903=VERTEX_POINT('',#26048);
#6904=VERTEX_POINT('',#26061);
#6905=VERTEX_POINT('',#26065);
#6906=VERTEX_POINT('',#26066);
#6907=VERTEX_POINT('',#26070);
#6908=VERTEX_POINT('',#26072);
#6909=VERTEX_POINT('',#26076);
#6910=VERTEX_POINT('',#26078);
#6911=VERTEX_POINT('',#26092);
#6912=VERTEX_POINT('',#26093);
#6913=VERTEX_POINT('',#26095);
#6914=VERTEX_POINT('',#26097);
#6915=VERTEX_POINT('',#26103);
#6916=VERTEX_POINT('',#26105);
#6917=VERTEX_POINT('',#26118);
#6918=VERTEX_POINT('',#26122);
#6919=VERTEX_POINT('',#26124);
#6920=VERTEX_POINT('',#26130);
#6921=VERTEX_POINT('',#26131);
#6922=VERTEX_POINT('',#26133);
#6923=VERTEX_POINT('',#26135);
#6924=VERTEX_POINT('',#26139);
#6925=VERTEX_POINT('',#26145);
#6926=VERTEX_POINT('',#26147);
#6927=VERTEX_POINT('',#26160);
#6928=VERTEX_POINT('',#26164);
#6929=VERTEX_POINT('',#26166);
#6930=VERTEX_POINT('',#26172);
#6931=VERTEX_POINT('',#26173);
#6932=VERTEX_POINT('',#26175);
#6933=VERTEX_POINT('',#26177);
#6934=VERTEX_POINT('',#26181);
#6935=VERTEX_POINT('',#26187);
#6936=VERTEX_POINT('',#26189);
#6937=VERTEX_POINT('',#26202);
#6938=VERTEX_POINT('',#26206);
#6939=VERTEX_POINT('',#26208);
#6940=VERTEX_POINT('',#26214);
#6941=VERTEX_POINT('',#26215);
#6942=VERTEX_POINT('',#26217);
#6943=VERTEX_POINT('',#26219);
#6944=VERTEX_POINT('',#26223);
#6945=VERTEX_POINT('',#26229);
#6946=VERTEX_POINT('',#26231);
#6947=VERTEX_POINT('',#26244);
#6948=VERTEX_POINT('',#26248);
#6949=VERTEX_POINT('',#26249);
#6950=VERTEX_POINT('',#26251);
#6951=VERTEX_POINT('',#26253);
#6952=VERTEX_POINT('',#26284);
#6953=VERTEX_POINT('',#26302);
#6954=VERTEX_POINT('',#26303);
#6955=VERTEX_POINT('',#26307);
#6956=VERTEX_POINT('',#26309);
#6957=VERTEX_POINT('',#26311);
#6958=VERTEX_POINT('',#26317);
#6959=VERTEX_POINT('',#26319);
#6960=VERTEX_POINT('',#26332);
#6961=VERTEX_POINT('',#26336);
#6962=VERTEX_POINT('',#26338);
#6963=VERTEX_POINT('',#26344);
#6964=VERTEX_POINT('',#26346);
#6965=VERTEX_POINT('',#26355);
#6966=VERTEX_POINT('',#26357);
#6967=VERTEX_POINT('',#26359);
#6968=VERTEX_POINT('',#26365);
#6969=VERTEX_POINT('',#26367);
#6970=VERTEX_POINT('',#26376);
#6971=VERTEX_POINT('',#26380);
#6972=VERTEX_POINT('',#26382);
#6973=VERTEX_POINT('',#26388);
#6974=VERTEX_POINT('',#26389);
#6975=VERTEX_POINT('',#26393);
#6976=VERTEX_POINT('',#26395);
#6977=VERTEX_POINT('',#26397);
#6978=VERTEX_POINT('',#26403);
#6979=VERTEX_POINT('',#26405);
#6980=VERTEX_POINT('',#26418);
#6981=VERTEX_POINT('',#26422);
#6982=VERTEX_POINT('',#26424);
#6983=VERTEX_POINT('',#26430);
#6984=VERTEX_POINT('',#26431);
#6985=VERTEX_POINT('',#26435);
#6986=VERTEX_POINT('',#26437);
#6987=VERTEX_POINT('',#26439);
#6988=VERTEX_POINT('',#26445);
#6989=VERTEX_POINT('',#26447);
#6990=VERTEX_POINT('',#26460);
#6991=VERTEX_POINT('',#26464);
#6992=VERTEX_POINT('',#26466);
#6993=VERTEX_POINT('',#26472);
#6994=VERTEX_POINT('',#26473);
#6995=VERTEX_POINT('',#26477);
#6996=VERTEX_POINT('',#26479);
#6997=VERTEX_POINT('',#26481);
#6998=VERTEX_POINT('',#26487);
#6999=VERTEX_POINT('',#26489);
#7000=VERTEX_POINT('',#26502);
#7001=VERTEX_POINT('',#26506);
#7002=VERTEX_POINT('',#26508);
#7003=VERTEX_POINT('',#26514);
#7004=VERTEX_POINT('',#26515);
#7005=VERTEX_POINT('',#26519);
#7006=VERTEX_POINT('',#26521);
#7007=VERTEX_POINT('',#26523);
#7008=VERTEX_POINT('',#26529);
#7009=VERTEX_POINT('',#26531);
#7010=VERTEX_POINT('',#26544);
#7011=VERTEX_POINT('',#26548);
#7012=VERTEX_POINT('',#26549);
#7013=VERTEX_POINT('',#26553);
#7014=VERTEX_POINT('',#26555);
#7015=VERTEX_POINT('',#26559);
#7016=VERTEX_POINT('',#26561);
#7017=VERTEX_POINT('',#26575);
#7018=VERTEX_POINT('',#26576);
#7019=VERTEX_POINT('',#26578);
#7020=VERTEX_POINT('',#26580);
#7021=VERTEX_POINT('',#26586);
#7022=VERTEX_POINT('',#26588);
#7023=VERTEX_POINT('',#26601);
#7024=VERTEX_POINT('',#26605);
#7025=VERTEX_POINT('',#26607);
#7026=VERTEX_POINT('',#26613);
#7027=VERTEX_POINT('',#26614);
#7028=VERTEX_POINT('',#26616);
#7029=VERTEX_POINT('',#26618);
#7030=VERTEX_POINT('',#26622);
#7031=VERTEX_POINT('',#26628);
#7032=VERTEX_POINT('',#26630);
#7033=VERTEX_POINT('',#26643);
#7034=VERTEX_POINT('',#26647);
#7035=VERTEX_POINT('',#26649);
#7036=VERTEX_POINT('',#26655);
#7037=VERTEX_POINT('',#26656);
#7038=VERTEX_POINT('',#26658);
#7039=VERTEX_POINT('',#26660);
#7040=VERTEX_POINT('',#26664);
#7041=VERTEX_POINT('',#26670);
#7042=VERTEX_POINT('',#26672);
#7043=VERTEX_POINT('',#26685);
#7044=VERTEX_POINT('',#26689);
#7045=VERTEX_POINT('',#26690);
#7046=VERTEX_POINT('',#26692);
#7047=VERTEX_POINT('',#26694);
#7048=VERTEX_POINT('',#26727);
#7049=VERTEX_POINT('',#26741);
#7050=VERTEX_POINT('',#26742);
#7051=VERTEX_POINT('',#26746);
#7052=VERTEX_POINT('',#26748);
#7053=VERTEX_POINT('',#26750);
#7054=VERTEX_POINT('',#26756);
#7055=VERTEX_POINT('',#26758);
#7056=VERTEX_POINT('',#26771);
#7057=VERTEX_POINT('',#26775);
#7058=VERTEX_POINT('',#26777);
#7059=VERTEX_POINT('',#26783);
#7060=VERTEX_POINT('',#26784);
#7061=VERTEX_POINT('',#26788);
#7062=VERTEX_POINT('',#26790);
#7063=VERTEX_POINT('',#26792);
#7064=VERTEX_POINT('',#26798);
#7065=VERTEX_POINT('',#26800);
#7066=VERTEX_POINT('',#26813);
#7067=VERTEX_POINT('',#26817);
#7068=VERTEX_POINT('',#26819);
#7069=VERTEX_POINT('',#26825);
#7070=VERTEX_POINT('',#26826);
#7071=VERTEX_POINT('',#26830);
#7072=VERTEX_POINT('',#26832);
#7073=VERTEX_POINT('',#26834);
#7074=VERTEX_POINT('',#26840);
#7075=VERTEX_POINT('',#26842);
#7076=VERTEX_POINT('',#26855);
#7077=VERTEX_POINT('',#26859);
#7078=VERTEX_POINT('',#26861);
#7079=VERTEX_POINT('',#26867);
#7080=VERTEX_POINT('',#26868);
#7081=VERTEX_POINT('',#26872);
#7082=VERTEX_POINT('',#26874);
#7083=VERTEX_POINT('',#26876);
#7084=VERTEX_POINT('',#26882);
#7085=VERTEX_POINT('',#26884);
#7086=VERTEX_POINT('',#26897);
#7087=VERTEX_POINT('',#26901);
#7088=VERTEX_POINT('',#26903);
#7089=VERTEX_POINT('',#26909);
#7090=VERTEX_POINT('',#26910);
#7091=VERTEX_POINT('',#26914);
#7092=VERTEX_POINT('',#26916);
#7093=VERTEX_POINT('',#26918);
#7094=VERTEX_POINT('',#26924);
#7095=VERTEX_POINT('',#26926);
#7096=VERTEX_POINT('',#26939);
#7097=VERTEX_POINT('',#26943);
#7098=VERTEX_POINT('',#26945);
#7099=VERTEX_POINT('',#26951);
#7100=VERTEX_POINT('',#26952);
#7101=VERTEX_POINT('',#26956);
#7102=VERTEX_POINT('',#26958);
#7103=VERTEX_POINT('',#26960);
#7104=VERTEX_POINT('',#26966);
#7105=VERTEX_POINT('',#26968);
#7106=VERTEX_POINT('',#26981);
#7107=VERTEX_POINT('',#26985);
#7108=VERTEX_POINT('',#26987);
#7109=VERTEX_POINT('',#26993);
#7110=VERTEX_POINT('',#26994);
#7111=VERTEX_POINT('',#26998);
#7112=VERTEX_POINT('',#27000);
#7113=VERTEX_POINT('',#27002);
#7114=VERTEX_POINT('',#27008);
#7115=VERTEX_POINT('',#27010);
#7116=VERTEX_POINT('',#27023);
#7117=VERTEX_POINT('',#27027);
#7118=VERTEX_POINT('',#27028);
#7119=VERTEX_POINT('',#27032);
#7120=VERTEX_POINT('',#27034);
#7121=VERTEX_POINT('',#27038);
#7122=VERTEX_POINT('',#27040);
#7123=VERTEX_POINT('',#27054);
#7124=VERTEX_POINT('',#27055);
#7125=VERTEX_POINT('',#27057);
#7126=VERTEX_POINT('',#27059);
#7127=VERTEX_POINT('',#27065);
#7128=VERTEX_POINT('',#27067);
#7129=VERTEX_POINT('',#27080);
#7130=VERTEX_POINT('',#27084);
#7131=VERTEX_POINT('',#27086);
#7132=VERTEX_POINT('',#27092);
#7133=VERTEX_POINT('',#27093);
#7134=VERTEX_POINT('',#27095);
#7135=VERTEX_POINT('',#27097);
#7136=VERTEX_POINT('',#27101);
#7137=VERTEX_POINT('',#27107);
#7138=VERTEX_POINT('',#27109);
#7139=VERTEX_POINT('',#27122);
#7140=VERTEX_POINT('',#27126);
#7141=VERTEX_POINT('',#27127);
#7142=VERTEX_POINT('',#27129);
#7143=VERTEX_POINT('',#27131);
#7144=VERTEX_POINT('',#27170);
#7145=VERTEX_POINT('',#27180);
#7146=VERTEX_POINT('',#27181);
#7147=VERTEX_POINT('',#27185);
#7148=VERTEX_POINT('',#27187);
#7149=VERTEX_POINT('',#27189);
#7150=VERTEX_POINT('',#27195);
#7151=VERTEX_POINT('',#27197);
#7152=VERTEX_POINT('',#27210);
#7153=VERTEX_POINT('',#27214);
#7154=VERTEX_POINT('',#27216);
#7155=VERTEX_POINT('',#27222);
#7156=VERTEX_POINT('',#27223);
#7157=VERTEX_POINT('',#27227);
#7158=VERTEX_POINT('',#27229);
#7159=VERTEX_POINT('',#27231);
#7160=VERTEX_POINT('',#27237);
#7161=VERTEX_POINT('',#27239);
#7162=VERTEX_POINT('',#27252);
#7163=VERTEX_POINT('',#27256);
#7164=VERTEX_POINT('',#27258);
#7165=VERTEX_POINT('',#27264);
#7166=VERTEX_POINT('',#27265);
#7167=VERTEX_POINT('',#27269);
#7168=VERTEX_POINT('',#27271);
#7169=VERTEX_POINT('',#27273);
#7170=VERTEX_POINT('',#27279);
#7171=VERTEX_POINT('',#27281);
#7172=VERTEX_POINT('',#27294);
#7173=VERTEX_POINT('',#27298);
#7174=VERTEX_POINT('',#27300);
#7175=VERTEX_POINT('',#27306);
#7176=VERTEX_POINT('',#27307);
#7177=VERTEX_POINT('',#27311);
#7178=VERTEX_POINT('',#27313);
#7179=VERTEX_POINT('',#27315);
#7180=VERTEX_POINT('',#27321);
#7181=VERTEX_POINT('',#27323);
#7182=VERTEX_POINT('',#27336);
#7183=VERTEX_POINT('',#27340);
#7184=VERTEX_POINT('',#27342);
#7185=VERTEX_POINT('',#27348);
#7186=VERTEX_POINT('',#27349);
#7187=VERTEX_POINT('',#27353);
#7188=VERTEX_POINT('',#27355);
#7189=VERTEX_POINT('',#27357);
#7190=VERTEX_POINT('',#27363);
#7191=VERTEX_POINT('',#27365);
#7192=VERTEX_POINT('',#27378);
#7193=VERTEX_POINT('',#27382);
#7194=VERTEX_POINT('',#27384);
#7195=VERTEX_POINT('',#27390);
#7196=VERTEX_POINT('',#27391);
#7197=VERTEX_POINT('',#27395);
#7198=VERTEX_POINT('',#27397);
#7199=VERTEX_POINT('',#27399);
#7200=VERTEX_POINT('',#27405);
#7201=VERTEX_POINT('',#27407);
#7202=VERTEX_POINT('',#27420);
#7203=VERTEX_POINT('',#27424);
#7204=VERTEX_POINT('',#27426);
#7205=VERTEX_POINT('',#27432);
#7206=VERTEX_POINT('',#27433);
#7207=VERTEX_POINT('',#27437);
#7208=VERTEX_POINT('',#27439);
#7209=VERTEX_POINT('',#27441);
#7210=VERTEX_POINT('',#27447);
#7211=VERTEX_POINT('',#27449);
#7212=VERTEX_POINT('',#27462);
#7213=VERTEX_POINT('',#27466);
#7214=VERTEX_POINT('',#27468);
#7215=VERTEX_POINT('',#27474);
#7216=VERTEX_POINT('',#27475);
#7217=VERTEX_POINT('',#27479);
#7218=VERTEX_POINT('',#27481);
#7219=VERTEX_POINT('',#27483);
#7220=VERTEX_POINT('',#27489);
#7221=VERTEX_POINT('',#27491);
#7222=VERTEX_POINT('',#27504);
#7223=VERTEX_POINT('',#27508);
#7224=VERTEX_POINT('',#27509);
#7225=VERTEX_POINT('',#27513);
#7226=VERTEX_POINT('',#27515);
#7227=VERTEX_POINT('',#27519);
#7228=VERTEX_POINT('',#27521);
#7229=VERTEX_POINT('',#27535);
#7230=VERTEX_POINT('',#27536);
#7231=VERTEX_POINT('',#27538);
#7232=VERTEX_POINT('',#27540);
#7233=VERTEX_POINT('',#27546);
#7234=VERTEX_POINT('',#27548);
#7235=VERTEX_POINT('',#27561);
#7236=VERTEX_POINT('',#27565);
#7237=VERTEX_POINT('',#27566);
#7238=VERTEX_POINT('',#27568);
#7239=VERTEX_POINT('',#27570);
#7240=VERTEX_POINT('',#27613);
#7241=VERTEX_POINT('',#27619);
#7242=VERTEX_POINT('',#27620);
#7243=VERTEX_POINT('',#27622);
#7244=VERTEX_POINT('',#27629);
#7245=VERTEX_POINT('',#27631);
#7246=VERTEX_POINT('',#27640);
#7247=VERTEX_POINT('',#27644);
#7248=VERTEX_POINT('',#27646);
#7249=VERTEX_POINT('',#27652);
#7250=VERTEX_POINT('',#27653);
#7251=VERTEX_POINT('',#27655);
#7252=VERTEX_POINT('',#27657);
#7253=VERTEX_POINT('',#27661);
#7254=VERTEX_POINT('',#27667);
#7255=VERTEX_POINT('',#27669);
#7256=VERTEX_POINT('',#27682);
#7257=VERTEX_POINT('',#27686);
#7258=VERTEX_POINT('',#27688);
#7259=VERTEX_POINT('',#27694);
#7260=VERTEX_POINT('',#27695);
#7261=VERTEX_POINT('',#27697);
#7262=VERTEX_POINT('',#27699);
#7263=VERTEX_POINT('',#27703);
#7264=VERTEX_POINT('',#27709);
#7265=VERTEX_POINT('',#27711);
#7266=VERTEX_POINT('',#27724);
#7267=VERTEX_POINT('',#27728);
#7268=VERTEX_POINT('',#27730);
#7269=VERTEX_POINT('',#27736);
#7270=VERTEX_POINT('',#27737);
#7271=VERTEX_POINT('',#27739);
#7272=VERTEX_POINT('',#27741);
#7273=VERTEX_POINT('',#27745);
#7274=VERTEX_POINT('',#27751);
#7275=VERTEX_POINT('',#27753);
#7276=VERTEX_POINT('',#27766);
#7277=VERTEX_POINT('',#27770);
#7278=VERTEX_POINT('',#27772);
#7279=VERTEX_POINT('',#27778);
#7280=VERTEX_POINT('',#27779);
#7281=VERTEX_POINT('',#27781);
#7282=VERTEX_POINT('',#27783);
#7283=VERTEX_POINT('',#27787);
#7284=VERTEX_POINT('',#27793);
#7285=VERTEX_POINT('',#27795);
#7286=VERTEX_POINT('',#27808);
#7287=VERTEX_POINT('',#27812);
#7288=VERTEX_POINT('',#27814);
#7289=VERTEX_POINT('',#27820);
#7290=VERTEX_POINT('',#27821);
#7291=VERTEX_POINT('',#27823);
#7292=VERTEX_POINT('',#27825);
#7293=VERTEX_POINT('',#27829);
#7294=VERTEX_POINT('',#27835);
#7295=VERTEX_POINT('',#27837);
#7296=VERTEX_POINT('',#27850);
#7297=VERTEX_POINT('',#27854);
#7298=VERTEX_POINT('',#27856);
#7299=VERTEX_POINT('',#27862);
#7300=VERTEX_POINT('',#27863);
#7301=VERTEX_POINT('',#27865);
#7302=VERTEX_POINT('',#27867);
#7303=VERTEX_POINT('',#27871);
#7304=VERTEX_POINT('',#27877);
#7305=VERTEX_POINT('',#27879);
#7306=VERTEX_POINT('',#27892);
#7307=VERTEX_POINT('',#27896);
#7308=VERTEX_POINT('',#27898);
#7309=VERTEX_POINT('',#27904);
#7310=VERTEX_POINT('',#27905);
#7311=VERTEX_POINT('',#27907);
#7312=VERTEX_POINT('',#27909);
#7313=VERTEX_POINT('',#27913);
#7314=VERTEX_POINT('',#27919);
#7315=VERTEX_POINT('',#27921);
#7316=VERTEX_POINT('',#27934);
#7317=VERTEX_POINT('',#27938);
#7318=VERTEX_POINT('',#27940);
#7319=VERTEX_POINT('',#27946);
#7320=VERTEX_POINT('',#27947);
#7321=VERTEX_POINT('',#27949);
#7322=VERTEX_POINT('',#27951);
#7323=VERTEX_POINT('',#27955);
#7324=VERTEX_POINT('',#27961);
#7325=VERTEX_POINT('',#27963);
#7326=VERTEX_POINT('',#27976);
#7327=VERTEX_POINT('',#27980);
#7328=VERTEX_POINT('',#27982);
#7329=VERTEX_POINT('',#27988);
#7330=VERTEX_POINT('',#27990);
#7331=VERTEX_POINT('',#28032);
#7332=VERTEX_POINT('',#28036);
#7333=VERTEX_POINT('',#28040);
#7334=VERTEX_POINT('',#28078);
#7335=VERTEX_POINT('',#28080);
#7336=VERTEX_POINT('',#28086);
#7337=VERTEX_POINT('',#28088);
#7338=VERTEX_POINT('',#28095);
#7339=VERTEX_POINT('',#28097);
#7340=VERTEX_POINT('',#28107);
#7341=VERTEX_POINT('',#28109);
#7342=VERTEX_POINT('',#28113);
#7343=VERTEX_POINT('',#28115);
#7344=VERTEX_POINT('',#28122);
#7345=VERTEX_POINT('',#28123);
#7346=VERTEX_POINT('',#28125);
#7347=VERTEX_POINT('',#28127);
#7348=VERTEX_POINT('',#28134);
#7349=VERTEX_POINT('',#28145);
#7350=VERTEX_POINT('',#28149);
#7351=VERTEX_POINT('',#28154);
#7352=VERTEX_POINT('',#28158);
#7353=VERTEX_POINT('',#28160);
#7354=VERTEX_POINT('',#28167);
#7355=VERTEX_POINT('',#28169);
#7356=VERTEX_POINT('',#28179);
#7357=VERTEX_POINT('',#28181);
#7358=VERTEX_POINT('',#28185);
#7359=VERTEX_POINT('',#28187);
#7360=VERTEX_POINT('',#28194);
#7361=VERTEX_POINT('',#28195);
#7362=VERTEX_POINT('',#28197);
#7363=VERTEX_POINT('',#28199);
#7364=VERTEX_POINT('',#28206);
#7365=VERTEX_POINT('',#28217);
#7366=VERTEX_POINT('',#28221);
#7367=VERTEX_POINT('',#28226);
#7368=VERTEX_POINT('',#28230);
#7369=VERTEX_POINT('',#28232);
#7370=VERTEX_POINT('',#28239);
#7371=VERTEX_POINT('',#28241);
#7372=VERTEX_POINT('',#28251);
#7373=VERTEX_POINT('',#28253);
#7374=VERTEX_POINT('',#28257);
#7375=VERTEX_POINT('',#28259);
#7376=VERTEX_POINT('',#28266);
#7377=VERTEX_POINT('',#28268);
#7378=VERTEX_POINT('',#28275);
#7379=VERTEX_POINT('',#28282);
#7380=VERTEX_POINT('',#28286);
#7381=VERTEX_POINT('',#28288);
#7382=VERTEX_POINT('',#28292);
#7383=VERTEX_POINT('',#28295);
#7384=VERTEX_POINT('',#28399);
#7385=VERTEX_POINT('',#28401);
#7386=VERTEX_POINT('',#28405);
#7387=VERTEX_POINT('',#28407);
#7388=VERTEX_POINT('',#28409);
#7389=VERTEX_POINT('',#28411);
#7390=VERTEX_POINT('',#28413);
#7391=VERTEX_POINT('',#28415);
#7392=VERTEX_POINT('',#28418);
#7393=VERTEX_POINT('',#28422);
#7394=VERTEX_POINT('',#28426);
#7395=VERTEX_POINT('',#28430);
#7396=VERTEX_POINT('',#28434);
#7397=VERTEX_POINT('',#28438);
#7398=VERTEX_POINT('',#28442);
#7399=VERTEX_POINT('',#28446);
#7400=VERTEX_POINT('',#28450);
#7401=VERTEX_POINT('',#28454);
#7402=VERTEX_POINT('',#28572);
#7403=VERTEX_POINT('',#28574);
#7404=VERTEX_POINT('',#28577);
#7405=VERTEX_POINT('',#28579);
#7406=VERTEX_POINT('',#28582);
#7407=VERTEX_POINT('',#28584);
#7408=VERTEX_POINT('',#28587);
#7409=VERTEX_POINT('',#28589);
#7410=VERTEX_POINT('',#28592);
#7411=VERTEX_POINT('',#28594);
#7412=VERTEX_POINT('',#28597);
#7413=VERTEX_POINT('',#28603);
#7414=VERTEX_POINT('',#28604);
#7415=VERTEX_POINT('',#28606);
#7416=VERTEX_POINT('',#28632);
#7417=VERTEX_POINT('',#28672);
#7418=VERTEX_POINT('',#28673);
#7419=VERTEX_POINT('',#28759);
#7420=VERTEX_POINT('',#28760);
#7421=VERTEX_POINT('',#28849);
#7422=VERTEX_POINT('',#28850);
#7423=VERTEX_POINT('',#28936);
#7424=VERTEX_POINT('',#28937);
#7425=VERTEX_POINT('',#29023);
#7426=VERTEX_POINT('',#29024);
#7427=VERTEX_POINT('',#29113);
#7428=VERTEX_POINT('',#29114);
#7429=VERTEX_POINT('',#29200);
#7430=VERTEX_POINT('',#29201);
#7431=VERTEX_POINT('',#29287);
#7432=VERTEX_POINT('',#29288);
#7433=VERTEX_POINT('',#29377);
#7434=VERTEX_POINT('',#29378);
#7435=VERTEX_POINT('',#29464);
#7436=VERTEX_POINT('',#29465);
#7437=VERTEX_POINT('',#29551);
#7438=VERTEX_POINT('',#29552);
#7439=VERTEX_POINT('',#29554);
#7440=VERTEX_POINT('',#29562);
#7441=VERTEX_POINT('',#29581);
#7442=VERTEX_POINT('',#29582);
#7443=VERTEX_POINT('',#29584);
#7444=VERTEX_POINT('',#29597);
#7445=VERTEX_POINT('',#29614);
#7446=VERTEX_POINT('',#29615);
#7447=VERTEX_POINT('',#29651);
#7448=VERTEX_POINT('',#29652);
#7449=VERTEX_POINT('',#29689);
#7450=VERTEX_POINT('',#29690);
#7451=VERTEX_POINT('',#29726);
#7452=VERTEX_POINT('',#29727);
#7453=VERTEX_POINT('',#29763);
#7454=VERTEX_POINT('',#29764);
#7455=VERTEX_POINT('',#29801);
#7456=VERTEX_POINT('',#29802);
#7457=VERTEX_POINT('',#29838);
#7458=VERTEX_POINT('',#29839);
#7459=VERTEX_POINT('',#29875);
#7460=VERTEX_POINT('',#29876);
#7461=VERTEX_POINT('',#29913);
#7462=VERTEX_POINT('',#29914);
#7463=VERTEX_POINT('',#29950);
#7464=VERTEX_POINT('',#29951);
#7465=VERTEX_POINT('',#29987);
#7466=VERTEX_POINT('',#29988);
#7467=VERTEX_POINT('',#29990);
#7468=VERTEX_POINT('',#29997);
#7469=VERTEX_POINT('',#31878);
#7470=VERTEX_POINT('',#31882);
#7471=VERTEX_POINT('',#31886);
#7472=VERTEX_POINT('',#31889);
#7473=VERTEX_POINT('',#31893);
#7474=VERTEX_POINT('',#31899);
#7475=VERTEX_POINT('',#31900);
#7476=VERTEX_POINT('',#31902);
#7477=VERTEX_POINT('',#31913);
#7478=VERTEX_POINT('',#31923);
#7479=VERTEX_POINT('',#31924);
#7480=VERTEX_POINT('',#31971);
#7481=VERTEX_POINT('',#31972);
#7482=VERTEX_POINT('',#32022);
#7483=VERTEX_POINT('',#32023);
#7484=VERTEX_POINT('',#32073);
#7485=VERTEX_POINT('',#32074);
#7486=VERTEX_POINT('',#32121);
#7487=VERTEX_POINT('',#32122);
#7488=VERTEX_POINT('',#32175);
#7489=VERTEX_POINT('',#32176);
#7490=VERTEX_POINT('',#32178);
#7491=VERTEX_POINT('',#32185);
#7492=VERTEX_POINT('',#32193);
#7493=VERTEX_POINT('',#32194);
#7494=VERTEX_POINT('',#32218);
#7495=VERTEX_POINT('',#32219);
#7496=VERTEX_POINT('',#32243);
#7497=VERTEX_POINT('',#32244);
#7498=VERTEX_POINT('',#32267);
#7499=VERTEX_POINT('',#32268);
#7500=VERTEX_POINT('',#32293);
#7501=VERTEX_POINT('',#32294);
#7502=VERTEX_POINT('',#32317);
#7503=VERTEX_POINT('',#32406);
#7504=VERTEX_POINT('',#32408);
#7505=VERTEX_POINT('',#32702);
#7506=VERTEX_POINT('',#32801);
#7507=VERTEX_POINT('',#33103);
#7508=VERTEX_POINT('',#33106);
#7509=VERTEX_POINT('',#33110);
#7510=VERTEX_POINT('',#33115);
#7511=VERTEX_POINT('',#33121);
#7512=VERTEX_POINT('',#33122);
#7513=VERTEX_POINT('',#33125);
#7514=VERTEX_POINT('',#33127);
#7515=VERTEX_POINT('',#33131);
#7516=VERTEX_POINT('',#33135);
#7517=VERTEX_POINT('',#33139);
#7518=VERTEX_POINT('',#33141);
#7519=VERTEX_POINT('',#33144);
#7520=VERTEX_POINT('',#33148);
#7521=VERTEX_POINT('',#33153);
#7522=VERTEX_POINT('',#33155);
#7523=VERTEX_POINT('',#33159);
#7524=VERTEX_POINT('',#33167);
#7525=VERTEX_POINT('',#33169);
#7526=VERTEX_POINT('',#33173);
#7527=VERTEX_POINT('',#33176);
#7528=VERTEX_POINT('',#33182);
#7529=VERTEX_POINT('',#33184);
#7530=VERTEX_POINT('',#33186);
#7531=VERTEX_POINT('',#33190);
#7532=VERTEX_POINT('',#33194);
#7533=VERTEX_POINT('',#33197);
#7534=VERTEX_POINT('',#33201);
#7535=VERTEX_POINT('',#33207);
#7536=VERTEX_POINT('',#33209);
#7537=VERTEX_POINT('',#33213);
#7538=VERTEX_POINT('',#33217);
#7539=VERTEX_POINT('',#33220);
#7540=VERTEX_POINT('',#33224);
#7541=VERTEX_POINT('',#33227);
#7542=VERTEX_POINT('',#33229);
#7543=VERTEX_POINT('',#33249);
#7544=VERTEX_POINT('',#33251);
#7545=VERTEX_POINT('',#33283);
#7546=VERTEX_POINT('',#33285);
#7547=VERTEX_POINT('',#33317);
#7548=VERTEX_POINT('',#33319);
#7549=VERTEX_POINT('',#33351);
#7550=VERTEX_POINT('',#33353);
#7551=VERTEX_POINT('',#33385);
#7552=VERTEX_POINT('',#33387);
#7553=VERTEX_POINT('',#33419);
#7554=VERTEX_POINT('',#33457);
#7555=VERTEX_POINT('',#33462);
#7556=VERTEX_POINT('',#33469);
#7557=VERTEX_POINT('',#33475);
#7558=VERTEX_POINT('',#33506);
#7559=VERTEX_POINT('',#33511);
#7560=VERTEX_POINT('',#33518);
#7561=VERTEX_POINT('',#33541);
#7562=VERTEX_POINT('',#33551);
#7563=VERTEX_POINT('',#33561);
#7564=VERTEX_POINT('',#33595);
#7565=VERTEX_POINT('',#33602);
#7566=VERTEX_POINT('',#33617);
#7567=VERTEX_POINT('',#33628);
#7568=VERTEX_POINT('',#33635);
#7569=VERTEX_POINT('',#33644);
#7570=VERTEX_POINT('',#33653);
#7571=VERTEX_POINT('',#33660);
#7572=VERTEX_POINT('',#33694);
#7573=VERTEX_POINT('',#33695);
#7574=VERTEX_POINT('',#33727);
#7575=VERTEX_POINT('',#33728);
#7576=VERTEX_POINT('',#33735);
#7577=VERTEX_POINT('',#33736);
#7578=VERTEX_POINT('',#33768);
#7579=VERTEX_POINT('',#33769);
#7580=VERTEX_POINT('',#33776);
#7581=VERTEX_POINT('',#33777);
#7582=VERTEX_POINT('',#33784);
#7583=VERTEX_POINT('',#33785);
#7584=VERTEX_POINT('',#33804);
#7585=VERTEX_POINT('',#33823);
#7586=VERTEX_POINT('',#33824);
#7587=VERTEX_POINT('',#34520);
#7588=VERTEX_POINT('',#34522);
#7589=VERTEX_POINT('',#34591);
#7590=VERTEX_POINT('',#34592);
#7591=VERTEX_POINT('',#34594);
#7592=VERTEX_POINT('',#34605);
#7593=VERTEX_POINT('',#34615);
#7594=VERTEX_POINT('',#34616);
#7595=VERTEX_POINT('',#34663);
#7596=VERTEX_POINT('',#34664);
#7597=VERTEX_POINT('',#34711);
#7598=VERTEX_POINT('',#34712);
#7599=VERTEX_POINT('',#34759);
#7600=VERTEX_POINT('',#34760);
#7601=VERTEX_POINT('',#34762);
#7602=VERTEX_POINT('',#34770);
#7603=VERTEX_POINT('',#34778);
#7604=VERTEX_POINT('',#34779);
#7605=VERTEX_POINT('',#34803);
#7606=VERTEX_POINT('',#34804);
#7607=VERTEX_POINT('',#34827);
#7608=VERTEX_POINT('',#34828);
#7609=VERTEX_POINT('',#34851);
#7610=VERTEX_POINT('',#34940);
#7611=VERTEX_POINT('',#34942);
#7612=VERTEX_POINT('',#35178);
#7613=VERTEX_POINT('',#35277);
#7614=VERTEX_POINT('',#35280);
#7615=VERTEX_POINT('',#35523);
#7616=VERTEX_POINT('',#35524);
#7617=VERTEX_POINT('',#35526);
#7618=VERTEX_POINT('',#35528);
#7619=VERTEX_POINT('',#35532);
#7620=VERTEX_POINT('',#35534);
#7621=VERTEX_POINT('',#35538);
#7622=VERTEX_POINT('',#35540);
#7623=VERTEX_POINT('',#35544);
#7624=VERTEX_POINT('',#35546);
#7625=VERTEX_POINT('',#35550);
#7626=VERTEX_POINT('',#35552);
#7627=VERTEX_POINT('',#35560);
#7628=VERTEX_POINT('',#35567);
#7629=VERTEX_POINT('',#35573);
#7630=VERTEX_POINT('',#35574);
#7631=VERTEX_POINT('',#35576);
#7632=VERTEX_POINT('',#35587);
#7633=VERTEX_POINT('',#35597);
#7634=VERTEX_POINT('',#35598);
#7635=VERTEX_POINT('',#35645);
#7636=VERTEX_POINT('',#35646);
#7637=VERTEX_POINT('',#35693);
#7638=VERTEX_POINT('',#35694);
#7639=VERTEX_POINT('',#35747);
#7640=VERTEX_POINT('',#35748);
#7641=VERTEX_POINT('',#35795);
#7642=VERTEX_POINT('',#35796);
#7643=VERTEX_POINT('',#35843);
#7644=VERTEX_POINT('',#35844);
#7645=VERTEX_POINT('',#35891);
#7646=VERTEX_POINT('',#35892);
#7647=VERTEX_POINT('',#35945);
#7648=VERTEX_POINT('',#35946);
#7649=VERTEX_POINT('',#35993);
#7650=VERTEX_POINT('',#35994);
#7651=VERTEX_POINT('',#36041);
#7652=VERTEX_POINT('',#36042);
#7653=VERTEX_POINT('',#36095);
#7654=VERTEX_POINT('',#36096);
#7655=VERTEX_POINT('',#36143);
#7656=VERTEX_POINT('',#36144);
#7657=VERTEX_POINT('',#36191);
#7658=VERTEX_POINT('',#36192);
#7659=VERTEX_POINT('',#36245);
#7660=VERTEX_POINT('',#36246);
#7661=VERTEX_POINT('',#36293);
#7662=VERTEX_POINT('',#36294);
#7663=VERTEX_POINT('',#36296);
#7664=VERTEX_POINT('',#36306);
#7665=VERTEX_POINT('',#36317);
#7666=VERTEX_POINT('',#36318);
#7667=VERTEX_POINT('',#36342);
#7668=VERTEX_POINT('',#36343);
#7669=VERTEX_POINT('',#36367);
#7670=VERTEX_POINT('',#36368);
#7671=VERTEX_POINT('',#36391);
#7672=VERTEX_POINT('',#36392);
#7673=VERTEX_POINT('',#36416);
#7674=VERTEX_POINT('',#36417);
#7675=VERTEX_POINT('',#36441);
#7676=VERTEX_POINT('',#36442);
#7677=VERTEX_POINT('',#36465);
#7678=VERTEX_POINT('',#36466);
#7679=VERTEX_POINT('',#36490);
#7680=VERTEX_POINT('',#36491);
#7681=VERTEX_POINT('',#36515);
#7682=VERTEX_POINT('',#36516);
#7683=VERTEX_POINT('',#36539);
#7684=VERTEX_POINT('',#36540);
#7685=VERTEX_POINT('',#36563);
#7686=VERTEX_POINT('',#36564);
#7687=VERTEX_POINT('',#36588);
#7688=VERTEX_POINT('',#36589);
#7689=VERTEX_POINT('',#36613);
#7690=VERTEX_POINT('',#36614);
#7691=VERTEX_POINT('',#37024);
#7692=VERTEX_POINT('',#37123);
#7693=VERTEX_POINT('',#37219);
#7694=VERTEX_POINT('',#37222);
#7695=VERTEX_POINT('',#37709);
#7696=VERTEX_POINT('',#37803);
#7697=VERTEX_POINT('',#37804);
#7698=VERTEX_POINT('',#37808);
#7699=VERTEX_POINT('',#37810);
#7700=VERTEX_POINT('',#37814);
#7701=VERTEX_POINT('',#37818);
#7702=VERTEX_POINT('',#37824);
#7703=VERTEX_POINT('',#37826);
#7704=VERTEX_POINT('',#37828);
#7705=VERTEX_POINT('',#37830);
#7706=VERTEX_POINT('',#37832);
#7707=VERTEX_POINT('',#37834);
#7708=VERTEX_POINT('',#37836);
#7709=VERTEX_POINT('',#37838);
#7710=VERTEX_POINT('',#37840);
#7711=VERTEX_POINT('',#37842);
#7712=VERTEX_POINT('',#37844);
#7713=VERTEX_POINT('',#37846);
#7714=VERTEX_POINT('',#37848);
#7715=VERTEX_POINT('',#37850);
#7716=VERTEX_POINT('',#37852);
#7717=VERTEX_POINT('',#37854);
#7718=VERTEX_POINT('',#37856);
#7719=VERTEX_POINT('',#37858);
#7720=VERTEX_POINT('',#37860);
#7721=VERTEX_POINT('',#37862);
#7722=VERTEX_POINT('',#37864);
#7723=VERTEX_POINT('',#37866);
#7724=VERTEX_POINT('',#37868);
#7725=VERTEX_POINT('',#37870);
#7726=VERTEX_POINT('',#37872);
#7727=VERTEX_POINT('',#37874);
#7728=VERTEX_POINT('',#37876);
#7729=VERTEX_POINT('',#37878);
#7730=VERTEX_POINT('',#37880);
#7731=VERTEX_POINT('',#37882);
#7732=VERTEX_POINT('',#37884);
#7733=VERTEX_POINT('',#37886);
#7734=VERTEX_POINT('',#37888);
#7735=VERTEX_POINT('',#37890);
#7736=VERTEX_POINT('',#37892);
#7737=VERTEX_POINT('',#37894);
#7738=VERTEX_POINT('',#37896);
#7739=VERTEX_POINT('',#37898);
#7740=VERTEX_POINT('',#37900);
#7741=VERTEX_POINT('',#37902);
#7742=VERTEX_POINT('',#37904);
#7743=VERTEX_POINT('',#37906);
#7744=VERTEX_POINT('',#37908);
#7745=VERTEX_POINT('',#37910);
#7746=VERTEX_POINT('',#37912);
#7747=VERTEX_POINT('',#37914);
#7748=VERTEX_POINT('',#37916);
#7749=VERTEX_POINT('',#37918);
#7750=VERTEX_POINT('',#37920);
#7751=VERTEX_POINT('',#37922);
#7752=VERTEX_POINT('',#37924);
#7753=VERTEX_POINT('',#37926);
#7754=VERTEX_POINT('',#37928);
#7755=VERTEX_POINT('',#37930);
#7756=VERTEX_POINT('',#37932);
#7757=VERTEX_POINT('',#37934);
#7758=VERTEX_POINT('',#37937);
#7759=VERTEX_POINT('',#37939);
#7760=VERTEX_POINT('',#37941);
#7761=VERTEX_POINT('',#37943);
#7762=VERTEX_POINT('',#37945);
#7763=VERTEX_POINT('',#37947);
#7764=VERTEX_POINT('',#37949);
#7765=VERTEX_POINT('',#37951);
#7766=VERTEX_POINT('',#37953);
#7767=VERTEX_POINT('',#37955);
#7768=VERTEX_POINT('',#37957);
#7769=VERTEX_POINT('',#37959);
#7770=VERTEX_POINT('',#37961);
#7771=VERTEX_POINT('',#37963);
#7772=VERTEX_POINT('',#37965);
#7773=VERTEX_POINT('',#37967);
#7774=VERTEX_POINT('',#37969);
#7775=VERTEX_POINT('',#37971);
#7776=VERTEX_POINT('',#37973);
#7777=VERTEX_POINT('',#37975);
#7778=VERTEX_POINT('',#37977);
#7779=VERTEX_POINT('',#37979);
#7780=VERTEX_POINT('',#37981);
#7781=VERTEX_POINT('',#37983);
#7782=VERTEX_POINT('',#37985);
#7783=VERTEX_POINT('',#37987);
#7784=VERTEX_POINT('',#37989);
#7785=VERTEX_POINT('',#37991);
#7786=VERTEX_POINT('',#37993);
#7787=VERTEX_POINT('',#37995);
#7788=VERTEX_POINT('',#37997);
#7789=VERTEX_POINT('',#37999);
#7790=VERTEX_POINT('',#38001);
#7791=VERTEX_POINT('',#38003);
#7792=VERTEX_POINT('',#38005);
#7793=VERTEX_POINT('',#38007);
#7794=VERTEX_POINT('',#38009);
#7795=VERTEX_POINT('',#38011);
#7796=VERTEX_POINT('',#38013);
#7797=VERTEX_POINT('',#38015);
#7798=VERTEX_POINT('',#38017);
#7799=VERTEX_POINT('',#38019);
#7800=VERTEX_POINT('',#38021);
#7801=VERTEX_POINT('',#38023);
#7802=VERTEX_POINT('',#38025);
#7803=VERTEX_POINT('',#38027);
#7804=VERTEX_POINT('',#38029);
#7805=VERTEX_POINT('',#38031);
#7806=VERTEX_POINT('',#38033);
#7807=VERTEX_POINT('',#38035);
#7808=VERTEX_POINT('',#38037);
#7809=VERTEX_POINT('',#38039);
#7810=VERTEX_POINT('',#38041);
#7811=VERTEX_POINT('',#38043);
#7812=VERTEX_POINT('',#38045);
#7813=VERTEX_POINT('',#38047);
#7814=VERTEX_POINT('',#38049);
#7815=VERTEX_POINT('',#38051);
#7816=VERTEX_POINT('',#38053);
#7817=VERTEX_POINT('',#38055);
#7818=VERTEX_POINT('',#38057);
#7819=VERTEX_POINT('',#38059);
#7820=VERTEX_POINT('',#38063);
#7821=VERTEX_POINT('',#38067);
#7822=VERTEX_POINT('',#38077);
#7823=VERTEX_POINT('',#38081);
#7824=VERTEX_POINT('',#38091);
#7825=VERTEX_POINT('',#38095);
#7826=VERTEX_POINT('',#38105);
#7827=VERTEX_POINT('',#38109);
#7828=VERTEX_POINT('',#38119);
#7829=VERTEX_POINT('',#38123);
#7830=VERTEX_POINT('',#38133);
#7831=VERTEX_POINT('',#38137);
#7832=VERTEX_POINT('',#38147);
#7833=VERTEX_POINT('',#38151);
#7834=VERTEX_POINT('',#38161);
#7835=VERTEX_POINT('',#38165);
#7836=VERTEX_POINT('',#38175);
#7837=VERTEX_POINT('',#38179);
#7838=VERTEX_POINT('',#38189);
#7839=VERTEX_POINT('',#38193);
#7840=VERTEX_POINT('',#38203);
#7841=VERTEX_POINT('',#38207);
#7842=VERTEX_POINT('',#38217);
#7843=VERTEX_POINT('',#38221);
#7844=VERTEX_POINT('',#38231);
#7845=VERTEX_POINT('',#38235);
#7846=VERTEX_POINT('',#38245);
#7847=VERTEX_POINT('',#38249);
#7848=VERTEX_POINT('',#38259);
#7849=VERTEX_POINT('',#38263);
#7850=VERTEX_POINT('',#38273);
#7851=VERTEX_POINT('',#38277);
#7852=VERTEX_POINT('',#38287);
#7853=VERTEX_POINT('',#38291);
#7854=VERTEX_POINT('',#38301);
#7855=VERTEX_POINT('',#38305);
#7856=VERTEX_POINT('',#38315);
#7857=VERTEX_POINT('',#38319);
#7858=VERTEX_POINT('',#38329);
#7859=VERTEX_POINT('',#38333);
#7860=VERTEX_POINT('',#38343);
#7861=VERTEX_POINT('',#38347);
#7862=VERTEX_POINT('',#38357);
#7863=VERTEX_POINT('',#38361);
#7864=VERTEX_POINT('',#38371);
#7865=VERTEX_POINT('',#38375);
#7866=VERTEX_POINT('',#38385);
#7867=VERTEX_POINT('',#38389);
#7868=VERTEX_POINT('',#38399);
#7869=VERTEX_POINT('',#38403);
#7870=VERTEX_POINT('',#38413);
#7871=VERTEX_POINT('',#38417);
#7872=VERTEX_POINT('',#38427);
#7873=VERTEX_POINT('',#38431);
#7874=VERTEX_POINT('',#38441);
#7875=VERTEX_POINT('',#38445);
#7876=VERTEX_POINT('',#38455);
#7877=VERTEX_POINT('',#38459);
#7878=VERTEX_POINT('',#38469);
#7879=VERTEX_POINT('',#38476);
#7880=VERTEX_POINT('',#38481);
#7881=EDGE_CURVE('',#6241,#6242,#4291,.T.);
#7882=EDGE_CURVE('',#6242,#6243,#4292,.T.);
#7883=EDGE_CURVE('',#6243,#6244,#4293,.T.);
#7884=EDGE_CURVE('',#6241,#6244,#4294,.T.);
#7885=EDGE_CURVE('',#6245,#6246,#4295,.T.);
#7886=EDGE_CURVE('',#6246,#6247,#4296,.T.);
#7887=EDGE_CURVE('',#6247,#6248,#4297,.T.);
#7888=EDGE_CURVE('',#6248,#6245,#4298,.T.);
#7889=EDGE_CURVE('',#6244,#6247,#4299,.T.);
#7890=EDGE_CURVE('',#6246,#6241,#4300,.T.);
#7891=EDGE_CURVE('',#6242,#6245,#4301,.T.);
#7892=EDGE_CURVE('',#6248,#6243,#4302,.T.);
#7893=EDGE_CURVE('',#6248,#6249,#4303,.T.);
#7894=EDGE_CURVE('',#6249,#6250,#4304,.T.);
#7895=EDGE_CURVE('',#6243,#6250,#4305,.T.);
#7896=EDGE_CURVE('',#6247,#6251,#4306,.T.);
#7897=EDGE_CURVE('',#6251,#6249,#4307,.T.);
#7898=EDGE_CURVE('',#6252,#6253,#4308,.T.);
#7899=EDGE_CURVE('',#6254,#6252,#4309,.T.);
#7900=EDGE_CURVE('',#6255,#6254,#4310,.T.);
#7901=EDGE_CURVE('',#6256,#6255,#1477,.T.);
#7902=EDGE_CURVE('',#6253,#6256,#1478,.T.);
#7903=EDGE_CURVE('',#6257,#6258,#4311,.T.);
#7904=EDGE_CURVE('',#6259,#6257,#4312,.T.);
#7905=EDGE_CURVE('',#6260,#6259,#4313,.T.);
#7906=EDGE_CURVE('',#6258,#6260,#4314,.T.);
#7907=EDGE_CURVE('',#6261,#6262,#4315,.T.);
#7908=EDGE_CURVE('',#6263,#6261,#4316,.T.);
#7909=EDGE_CURVE('',#6264,#6263,#4317,.T.);
#7910=EDGE_CURVE('',#6262,#6264,#4318,.T.);
#7911=EDGE_CURVE('',#6265,#6266,#4319,.T.);
#7912=EDGE_CURVE('',#6267,#6265,#4320,.T.);
#7913=EDGE_CURVE('',#6268,#6267,#4321,.T.);
#7914=EDGE_CURVE('',#6266,#6268,#4322,.T.);
#7915=EDGE_CURVE('',#6269,#6270,#4323,.T.);
#7916=EDGE_CURVE('',#6270,#6266,#4324,.F.);
#7917=EDGE_CURVE('',#6268,#6269,#4325,.T.);
#7918=EDGE_CURVE('',#6271,#6269,#4326,.T.);
#7919=EDGE_CURVE('',#6267,#6271,#4327,.T.);
#7920=EDGE_CURVE('',#6265,#6272,#4328,.F.);
#7921=EDGE_CURVE('',#6272,#6271,#4329,.T.);
#7922=EDGE_CURVE('',#6269,#6273,#4330,.T.);
#7923=EDGE_CURVE('',#6273,#6274,#4331,.T.);
#7924=EDGE_CURVE('',#6270,#6274,#4332,.T.);
#7925=EDGE_CURVE('',#6271,#6275,#4333,.T.);
#7926=EDGE_CURVE('',#6275,#6273,#4334,.T.);
#7927=EDGE_CURVE('',#6272,#6276,#4335,.T.);
#7928=EDGE_CURVE('',#6276,#6275,#4336,.T.);
#7929=EDGE_CURVE('',#6264,#6277,#4337,.F.);
#7930=EDGE_CURVE('',#6277,#6278,#4338,.T.);
#7931=EDGE_CURVE('',#6278,#6262,#4339,.F.);
#7932=EDGE_CURVE('',#6277,#6279,#4340,.T.);
#7933=EDGE_CURVE('',#6279,#6280,#4341,.T.);
#7934=EDGE_CURVE('',#6278,#6280,#4342,.T.);
#7935=EDGE_CURVE('',#6261,#6281,#4343,.F.);
#7936=EDGE_CURVE('',#6281,#6282,#4344,.T.);
#7937=EDGE_CURVE('',#6282,#6263,#4345,.F.);
#7938=EDGE_CURVE('',#6281,#6283,#4346,.T.);
#7939=EDGE_CURVE('',#6283,#6284,#4347,.T.);
#7940=EDGE_CURVE('',#6282,#6284,#4348,.T.);
#7941=EDGE_CURVE('',#6260,#6285,#4349,.F.);
#7942=EDGE_CURVE('',#6285,#6286,#4350,.T.);
#7943=EDGE_CURVE('',#6286,#6258,#4351,.F.);
#7944=EDGE_CURVE('',#6285,#6287,#4352,.T.);
#7945=EDGE_CURVE('',#6287,#6288,#4353,.T.);
#7946=EDGE_CURVE('',#6286,#6288,#4354,.T.);
#7947=EDGE_CURVE('',#6257,#6289,#4355,.F.);
#7948=EDGE_CURVE('',#6289,#6290,#4356,.T.);
#7949=EDGE_CURVE('',#6290,#6259,#4357,.F.);
#7950=EDGE_CURVE('',#6289,#6291,#4358,.T.);
#7951=EDGE_CURVE('',#6291,#6292,#4359,.T.);
#7952=EDGE_CURVE('',#6290,#6292,#4360,.T.);
#7953=EDGE_CURVE('',#6293,#6294,#4361,.T.);
#7954=EDGE_CURVE('',#6254,#6293,#4362,.T.);
#7955=EDGE_CURVE('',#6294,#6254,#4363,.T.);
#7956=EDGE_CURVE('',#6295,#6255,#1424,.F.);
#7957=EDGE_CURVE('',#6293,#6295,#4364,.T.);
#7958=EDGE_CURVE('',#6252,#6296,#4365,.T.);
#7959=EDGE_CURVE('',#6297,#6252,#4366,.T.);
#7960=EDGE_CURVE('',#6296,#6297,#4367,.T.);
#7961=EDGE_CURVE('',#6253,#6298,#1425,.F.);
#7962=EDGE_CURVE('',#6298,#6297,#4368,.T.);
#7963=EDGE_CURVE('',#6299,#6300,#4369,.T.);
#7964=EDGE_CURVE('',#6300,#6296,#4370,.T.);
#7965=EDGE_CURVE('',#6297,#6301,#4371,.T.);
#7966=EDGE_CURVE('',#6301,#6299,#4372,.T.);
#7967=EDGE_CURVE('',#6296,#6294,#4373,.T.);
#7968=EDGE_CURVE('',#6302,#6303,#4374,.T.);
#7969=EDGE_CURVE('',#6303,#6293,#4375,.T.);
#7970=EDGE_CURVE('',#6294,#6304,#4376,.T.);
#7971=EDGE_CURVE('',#6304,#6302,#4377,.T.);
#7972=EDGE_CURVE('',#6305,#6303,#4378,.T.);
#7973=EDGE_CURVE('',#6305,#6306,#1051,.T.);
#7974=EDGE_CURVE('',#6295,#6306,#1426,.T.);
#7975=EDGE_CURVE('',#6307,#6302,#4379,.T.);
#7976=EDGE_CURVE('',#6307,#6308,#4380,.T.);
#7977=EDGE_CURVE('',#6308,#6305,#1427,.T.);
#7978=EDGE_CURVE('',#6309,#6310,#428,.T.);
#7979=EDGE_CURVE('',#6310,#6306,#1479,.T.);
#7980=EDGE_CURVE('',#6308,#6309,#1480,.T.);
#7981=EDGE_CURVE('',#6311,#6309,#4381,.T.);
#7982=EDGE_CURVE('',#6312,#6311,#1428,.F.);
#7983=EDGE_CURVE('',#6312,#6313,#1481,.T.);
#7984=EDGE_CURVE('',#6314,#6313,#1429,.F.);
#7985=EDGE_CURVE('',#6315,#6314,#4382,.T.);
#7986=EDGE_CURVE('',#6316,#6315,#429,.T.);
#7987=EDGE_CURVE('',#6310,#6316,#430,.T.);
#7988=EDGE_CURVE('',#6317,#6307,#4383,.T.);
#7989=EDGE_CURVE('',#6318,#6317,#4384,.T.);
#7990=EDGE_CURVE('',#6315,#6318,#1482,.T.);
#7991=EDGE_CURVE('',#6311,#6314,#4385,.T.);
#7992=EDGE_CURVE('',#6319,#6319,#1483,.T.);
#7993=EDGE_CURVE('',#6320,#6320,#1484,.T.);
#7994=EDGE_CURVE('',#6321,#6322,#1052,.F.);
#7995=EDGE_CURVE('',#6322,#6316,#1485,.T.);
#7996=EDGE_CURVE('',#6318,#6321,#1430,.F.);
#7997=EDGE_CURVE('',#6270,#6272,#4386,.T.);
#7998=EDGE_CURVE('',#6274,#6276,#4387,.T.);
#7999=EDGE_CURVE('',#6278,#6281,#4388,.T.);
#8000=EDGE_CURVE('',#6280,#6283,#4389,.T.);
#8001=EDGE_CURVE('',#6282,#6277,#4390,.T.);
#8002=EDGE_CURVE('',#6284,#6279,#4391,.T.);
#8003=EDGE_CURVE('',#6286,#6289,#4392,.T.);
#8004=EDGE_CURVE('',#6288,#6291,#4393,.T.);
#8005=EDGE_CURVE('',#6290,#6285,#4394,.T.);
#8006=EDGE_CURVE('',#6292,#6287,#4395,.T.);
#8007=EDGE_CURVE('',#6319,#6323,#4396,.T.);
#8008=EDGE_CURVE('',#6323,#6323,#1486,.T.);
#8009=EDGE_CURVE('',#6323,#6324,#4397,.T.);
#8010=EDGE_CURVE('',#6324,#6324,#1487,.T.);
#8011=EDGE_CURVE('',#6301,#6321,#4398,.T.);
#8012=EDGE_CURVE('',#6317,#6299,#4399,.T.);
#8013=EDGE_CURVE('',#6322,#6298,#1431,.T.);
#8014=EDGE_CURVE('',#6304,#6300,#4400,.T.);
#8015=EDGE_CURVE('',#6313,#6312,#4401,.T.);
#8016=EDGE_CURVE('',#6325,#6325,#1488,.T.);
#8017=EDGE_CURVE('',#6326,#6326,#1489,.T.);
#8018=EDGE_CURVE('',#6326,#6327,#4402,.T.);
#8019=EDGE_CURVE('',#6327,#6327,#1490,.T.);
#8020=EDGE_CURVE('',#6328,#6328,#1491,.T.);
#8021=EDGE_CURVE('',#6328,#6326,#4403,.T.);
#8022=EDGE_CURVE('',#6327,#6256,#4404,.T.);
#8023=EDGE_CURVE('',#6320,#6329,#4405,.T.);
#8024=EDGE_CURVE('',#6329,#6329,#1492,.T.);
#8025=EDGE_CURVE('',#6330,#6330,#1493,.T.);
#8026=EDGE_CURVE('',#6330,#6329,#4406,.T.);
#8027=EDGE_CURVE('',#6328,#6331,#4407,.T.);
#8028=EDGE_CURVE('',#6331,#6331,#1494,.T.);
#8029=EDGE_CURVE('',#6332,#6332,#1495,.T.);
#8030=EDGE_CURVE('',#6333,#6333,#1496,.T.);
#8031=EDGE_CURVE('',#6334,#6334,#1497,.T.);
#8032=EDGE_CURVE('',#6332,#6330,#4408,.T.);
#8033=EDGE_CURVE('',#6325,#6335,#4409,.T.);
#8034=EDGE_CURVE('',#6335,#6335,#1498,.T.);
#8035=EDGE_CURVE('',#6336,#6336,#1499,.T.);
#8036=EDGE_CURVE('',#6334,#6336,#4410,.T.);
#8037=EDGE_CURVE('',#6333,#6337,#4411,.T.);
#8038=EDGE_CURVE('',#6337,#6337,#1500,.T.);
#8039=EDGE_CURVE('',#6244,#6338,#4412,.T.);
#8040=EDGE_CURVE('',#6338,#6251,#4413,.T.);
#8041=EDGE_CURVE('',#6250,#6338,#4414,.T.);
#8042=EDGE_CURVE('',#6339,#6340,#1053,.T.);
#8043=EDGE_CURVE('',#6340,#6341,#4415,.T.);
#8044=EDGE_CURVE('',#6341,#6342,#4416,.F.);
#8045=EDGE_CURVE('',#6342,#6339,#4417,.T.);
#8046=EDGE_CURVE('',#6343,#6340,#1501,.T.);
#8047=EDGE_CURVE('',#6344,#6343,#4418,.T.);
#8048=EDGE_CURVE('',#6341,#6344,#1502,.T.);
#8049=EDGE_CURVE('',#6345,#6339,#431,.T.);
#8050=EDGE_CURVE('',#6345,#6346,#1503,.T.);
#8051=EDGE_CURVE('',#6346,#6347,#432,.T.);
#8052=EDGE_CURVE('',#6343,#6347,#1054,.T.);
#8053=EDGE_CURVE('',#6348,#6349,#1055,.T.);
#8054=EDGE_CURVE('',#6349,#6350,#4419,.T.);
#8055=EDGE_CURVE('',#6350,#6351,#4420,.F.);
#8056=EDGE_CURVE('',#6351,#6352,#4421,.T.);
#8057=EDGE_CURVE('',#6352,#6348,#1056,.T.);
#8058=EDGE_CURVE('',#6353,#6349,#1504,.T.);
#8059=EDGE_CURVE('',#6354,#6353,#4422,.T.);
#8060=EDGE_CURVE('',#6350,#6354,#1505,.T.);
#8061=EDGE_CURVE('',#6348,#6355,#433,.T.);
#8062=EDGE_CURVE('',#6355,#6356,#1506,.T.);
#8063=EDGE_CURVE('',#6357,#6356,#434,.T.);
#8064=EDGE_CURVE('',#6353,#6357,#1057,.T.);
#8065=EDGE_CURVE('',#6354,#6358,#4423,.T.);
#8066=EDGE_CURVE('',#6357,#6358,#4424,.T.);
#8067=EDGE_CURVE('',#6359,#6356,#1507,.T.);
#8068=EDGE_CURVE('',#6359,#6360,#435,.T.);
#8069=EDGE_CURVE('',#6361,#6360,#4425,.T.);
#8070=EDGE_CURVE('',#6361,#6358,#1508,.T.);
#8071=EDGE_CURVE('',#6362,#6363,#1058,.T.);
#8072=EDGE_CURVE('',#6363,#6364,#4426,.T.);
#8073=EDGE_CURVE('',#6364,#6365,#4427,.F.);
#8074=EDGE_CURVE('',#6365,#6366,#4428,.T.);
#8075=EDGE_CURVE('',#6366,#6362,#1059,.T.);
#8076=EDGE_CURVE('',#6366,#6367,#1509,.T.);
#8077=EDGE_CURVE('',#6368,#6367,#1060,.T.);
#8078=EDGE_CURVE('',#6368,#6369,#436,.T.);
#8079=EDGE_CURVE('',#6369,#6370,#1510,.T.);
#8080=EDGE_CURVE('',#6362,#6370,#437,.T.);
#8081=EDGE_CURVE('',#6365,#6371,#1511,.T.);
#8082=EDGE_CURVE('',#6367,#6371,#4429,.T.);
#8083=EDGE_CURVE('',#6372,#6373,#4430,.T.);
#8084=EDGE_CURVE('',#6372,#6374,#4431,.T.);
#8085=EDGE_CURVE('',#6374,#6375,#1061,.T.);
#8086=EDGE_CURVE('',#6375,#6376,#1062,.T.);
#8087=EDGE_CURVE('',#6376,#6373,#4432,.T.);
#8088=EDGE_CURVE('',#6351,#6373,#1512,.T.);
#8089=EDGE_CURVE('',#6352,#6376,#1513,.T.);
#8090=EDGE_CURVE('',#6375,#6377,#438,.T.);
#8091=EDGE_CURVE('',#6377,#6355,#1514,.T.);
#8092=EDGE_CURVE('',#6378,#6379,#1063,.T.);
#8093=EDGE_CURVE('',#6379,#6380,#4433,.T.);
#8094=EDGE_CURVE('',#6380,#6381,#4434,.F.);
#8095=EDGE_CURVE('',#6381,#6382,#4435,.T.);
#8096=EDGE_CURVE('',#6382,#6378,#1064,.T.);
#8097=EDGE_CURVE('',#6382,#6383,#1515,.T.);
#8098=EDGE_CURVE('',#6384,#6383,#1065,.T.);
#8099=EDGE_CURVE('',#6384,#6385,#439,.T.);
#8100=EDGE_CURVE('',#6385,#6386,#1516,.T.);
#8101=EDGE_CURVE('',#6378,#6386,#440,.T.);
#8102=EDGE_CURVE('',#6381,#6387,#1517,.T.);
#8103=EDGE_CURVE('',#6383,#6387,#4436,.T.);
#8104=EDGE_CURVE('',#6388,#6371,#4437,.T.);
#8105=EDGE_CURVE('',#6388,#6389,#4438,.T.);
#8106=EDGE_CURVE('',#6389,#6368,#1066,.T.);
#8107=EDGE_CURVE('',#6390,#6387,#4439,.T.);
#8108=EDGE_CURVE('',#6390,#6391,#4440,.T.);
#8109=EDGE_CURVE('',#6391,#6384,#1067,.T.);
#8110=EDGE_CURVE('',#6392,#6393,#4441,.T.);
#8111=EDGE_CURVE('',#6392,#6394,#4442,.T.);
#8112=EDGE_CURVE('',#6394,#6395,#1068,.T.);
#8113=EDGE_CURVE('',#6395,#6393,#4443,.T.);
#8114=EDGE_CURVE('',#6395,#6396,#441,.T.);
#8115=EDGE_CURVE('',#6397,#6396,#1518,.T.);
#8116=EDGE_CURVE('',#6398,#6397,#442,.T.);
#8117=EDGE_CURVE('',#6399,#6398,#4444,.T.);
#8118=EDGE_CURVE('',#6399,#6393,#1519,.T.);
#8119=EDGE_CURVE('',#6394,#6400,#1520,.T.);
#8120=EDGE_CURVE('',#6400,#6401,#443,.T.);
#8121=EDGE_CURVE('',#6401,#6402,#444,.T.);
#8122=EDGE_CURVE('',#6402,#6396,#1521,.T.);
#8123=EDGE_CURVE('',#6403,#6404,#1069,.T.);
#8124=EDGE_CURVE('',#6404,#6405,#4445,.T.);
#8125=EDGE_CURVE('',#6405,#6406,#4446,.F.);
#8126=EDGE_CURVE('',#6406,#6407,#4447,.T.);
#8127=EDGE_CURVE('',#6407,#6403,#1070,.T.);
#8128=EDGE_CURVE('',#6408,#6404,#1522,.T.);
#8129=EDGE_CURVE('',#6409,#6408,#4448,.T.);
#8130=EDGE_CURVE('',#6405,#6409,#1523,.T.);
#8131=EDGE_CURVE('',#6403,#6410,#445,.T.);
#8132=EDGE_CURVE('',#6410,#6411,#1524,.T.);
#8133=EDGE_CURVE('',#6411,#6412,#446,.T.);
#8134=EDGE_CURVE('',#6408,#6412,#447,.T.);
#8135=EDGE_CURVE('',#6413,#6414,#4449,.T.);
#8136=EDGE_CURVE('',#6413,#6415,#4450,.T.);
#8137=EDGE_CURVE('',#6415,#6416,#1071,.T.);
#8138=EDGE_CURVE('',#6416,#6417,#1072,.T.);
#8139=EDGE_CURVE('',#6417,#6414,#4451,.T.);
#8140=EDGE_CURVE('',#6415,#6418,#1525,.T.);
#8141=EDGE_CURVE('',#6419,#6418,#1073,.T.);
#8142=EDGE_CURVE('',#6419,#6420,#448,.T.);
#8143=EDGE_CURVE('',#6420,#6421,#1526,.T.);
#8144=EDGE_CURVE('',#6416,#6421,#449,.T.);
#8145=EDGE_CURVE('',#6422,#6413,#1527,.T.);
#8146=EDGE_CURVE('',#6418,#6422,#4452,.T.);
#8147=EDGE_CURVE('',#6422,#6423,#4453,.F.);
#8148=EDGE_CURVE('',#6423,#6424,#4454,.T.);
#8149=EDGE_CURVE('',#6424,#6419,#1074,.T.);
#8150=EDGE_CURVE('',#6425,#6426,#4455,.T.);
#8151=EDGE_CURVE('',#6425,#6427,#4456,.T.);
#8152=EDGE_CURVE('',#6427,#6428,#1075,.T.);
#8153=EDGE_CURVE('',#6428,#6429,#1076,.T.);
#8154=EDGE_CURVE('',#6429,#6426,#4457,.T.);
#8155=EDGE_CURVE('',#6427,#6430,#1528,.T.);
#8156=EDGE_CURVE('',#6431,#6430,#1077,.T.);
#8157=EDGE_CURVE('',#6431,#6432,#450,.T.);
#8158=EDGE_CURVE('',#6432,#6433,#1529,.T.);
#8159=EDGE_CURVE('',#6428,#6433,#451,.T.);
#8160=EDGE_CURVE('',#6434,#6425,#1530,.T.);
#8161=EDGE_CURVE('',#6430,#6434,#4458,.T.);
#8162=EDGE_CURVE('',#6434,#6435,#4459,.F.);
#8163=EDGE_CURVE('',#6435,#6436,#4460,.T.);
#8164=EDGE_CURVE('',#6436,#6431,#1078,.T.);
#8165=EDGE_CURVE('',#6437,#6438,#4461,.T.);
#8166=EDGE_CURVE('',#6437,#6439,#4462,.T.);
#8167=EDGE_CURVE('',#6439,#6440,#1079,.T.);
#8168=EDGE_CURVE('',#6440,#6441,#1080,.T.);
#8169=EDGE_CURVE('',#6441,#6438,#4463,.T.);
#8170=EDGE_CURVE('',#6439,#6442,#1531,.T.);
#8171=EDGE_CURVE('',#6443,#6442,#1081,.T.);
#8172=EDGE_CURVE('',#6443,#6444,#452,.T.);
#8173=EDGE_CURVE('',#6444,#6445,#1532,.T.);
#8174=EDGE_CURVE('',#6440,#6445,#453,.T.);
#8175=EDGE_CURVE('',#6446,#6437,#1533,.T.);
#8176=EDGE_CURVE('',#6442,#6446,#4464,.T.);
#8177=EDGE_CURVE('',#6446,#6447,#4465,.F.);
#8178=EDGE_CURVE('',#6447,#6448,#4466,.T.);
#8179=EDGE_CURVE('',#6448,#6443,#1082,.T.);
#8180=EDGE_CURVE('',#6449,#6450,#4467,.T.);
#8181=EDGE_CURVE('',#6449,#6451,#4468,.T.);
#8182=EDGE_CURVE('',#6451,#6452,#1083,.T.);
#8183=EDGE_CURVE('',#6452,#6453,#1084,.T.);
#8184=EDGE_CURVE('',#6453,#6450,#4469,.T.);
#8185=EDGE_CURVE('',#6451,#6454,#1534,.T.);
#8186=EDGE_CURVE('',#6455,#6454,#1085,.T.);
#8187=EDGE_CURVE('',#6455,#6456,#454,.T.);
#8188=EDGE_CURVE('',#6456,#6457,#1535,.T.);
#8189=EDGE_CURVE('',#6452,#6457,#455,.T.);
#8190=EDGE_CURVE('',#6458,#6449,#1536,.T.);
#8191=EDGE_CURVE('',#6454,#6458,#4470,.T.);
#8192=EDGE_CURVE('',#6458,#6459,#4471,.F.);
#8193=EDGE_CURVE('',#6459,#6460,#4472,.T.);
#8194=EDGE_CURVE('',#6460,#6455,#1086,.T.);
#8195=EDGE_CURVE('',#6461,#6462,#4473,.T.);
#8196=EDGE_CURVE('',#6461,#6463,#4474,.T.);
#8197=EDGE_CURVE('',#6463,#6464,#1087,.T.);
#8198=EDGE_CURVE('',#6464,#6465,#1088,.T.);
#8199=EDGE_CURVE('',#6465,#6462,#4475,.T.);
#8200=EDGE_CURVE('',#6463,#6466,#1537,.T.);
#8201=EDGE_CURVE('',#6467,#6466,#1089,.T.);
#8202=EDGE_CURVE('',#6467,#6468,#456,.T.);
#8203=EDGE_CURVE('',#6468,#6469,#1538,.T.);
#8204=EDGE_CURVE('',#6464,#6469,#457,.T.);
#8205=EDGE_CURVE('',#6470,#6461,#1539,.T.);
#8206=EDGE_CURVE('',#6466,#6470,#4476,.T.);
#8207=EDGE_CURVE('',#6470,#6471,#4477,.F.);
#8208=EDGE_CURVE('',#6471,#6472,#4478,.T.);
#8209=EDGE_CURVE('',#6472,#6467,#1090,.T.);
#8210=EDGE_CURVE('',#6473,#6474,#4479,.T.);
#8211=EDGE_CURVE('',#6473,#6475,#4480,.T.);
#8212=EDGE_CURVE('',#6475,#6476,#1091,.T.);
#8213=EDGE_CURVE('',#6476,#6477,#1092,.T.);
#8214=EDGE_CURVE('',#6477,#6474,#4481,.T.);
#8215=EDGE_CURVE('',#6475,#6478,#1540,.T.);
#8216=EDGE_CURVE('',#6479,#6478,#1093,.T.);
#8217=EDGE_CURVE('',#6479,#6480,#458,.T.);
#8218=EDGE_CURVE('',#6480,#6481,#1541,.T.);
#8219=EDGE_CURVE('',#6476,#6481,#459,.T.);
#8220=EDGE_CURVE('',#6482,#6473,#1542,.T.);
#8221=EDGE_CURVE('',#6478,#6482,#4482,.T.);
#8222=EDGE_CURVE('',#6482,#6483,#4483,.F.);
#8223=EDGE_CURVE('',#6483,#6484,#4484,.T.);
#8224=EDGE_CURVE('',#6484,#6479,#1094,.T.);
#8225=EDGE_CURVE('',#6485,#6486,#4485,.T.);
#8226=EDGE_CURVE('',#6485,#6487,#4486,.T.);
#8227=EDGE_CURVE('',#6487,#6488,#1095,.T.);
#8228=EDGE_CURVE('',#6488,#6489,#1096,.T.);
#8229=EDGE_CURVE('',#6489,#6486,#4487,.T.);
#8230=EDGE_CURVE('',#6487,#6490,#1543,.T.);
#8231=EDGE_CURVE('',#6491,#6490,#1097,.T.);
#8232=EDGE_CURVE('',#6491,#6492,#460,.T.);
#8233=EDGE_CURVE('',#6492,#6493,#1544,.T.);
#8234=EDGE_CURVE('',#6488,#6493,#461,.T.);
#8235=EDGE_CURVE('',#6494,#6485,#1545,.T.);
#8236=EDGE_CURVE('',#6490,#6494,#4488,.T.);
#8237=EDGE_CURVE('',#6494,#6495,#4489,.F.);
#8238=EDGE_CURVE('',#6495,#6496,#4490,.T.);
#8239=EDGE_CURVE('',#6496,#6491,#1098,.T.);
#8240=EDGE_CURVE('',#6497,#6498,#4491,.T.);
#8241=EDGE_CURVE('',#6497,#6499,#4492,.T.);
#8242=EDGE_CURVE('',#6499,#6500,#1099,.T.);
#8243=EDGE_CURVE('',#6500,#6501,#1100,.T.);
#8244=EDGE_CURVE('',#6501,#6498,#4493,.T.);
#8245=EDGE_CURVE('',#6499,#6502,#1546,.T.);
#8246=EDGE_CURVE('',#6503,#6502,#1101,.T.);
#8247=EDGE_CURVE('',#6503,#6504,#462,.T.);
#8248=EDGE_CURVE('',#6504,#6505,#1547,.T.);
#8249=EDGE_CURVE('',#6500,#6505,#463,.T.);
#8250=EDGE_CURVE('',#6506,#6497,#1548,.T.);
#8251=EDGE_CURVE('',#6502,#6506,#4494,.T.);
#8252=EDGE_CURVE('',#6506,#6507,#4495,.F.);
#8253=EDGE_CURVE('',#6507,#6508,#4496,.T.);
#8254=EDGE_CURVE('',#6508,#6503,#1102,.T.);
#8255=EDGE_CURVE('',#6508,#6509,#1549,.T.);
#8256=EDGE_CURVE('',#6510,#6509,#1103,.T.);
#8257=EDGE_CURVE('',#6511,#6510,#464,.T.);
#8258=EDGE_CURVE('',#6511,#6504,#1550,.T.);
#8259=EDGE_CURVE('',#6370,#6377,#1551,.T.);
#8260=EDGE_CURVE('',#6374,#6363,#1552,.T.);
#8261=EDGE_CURVE('',#6386,#6369,#1553,.T.);
#8262=EDGE_CURVE('',#6389,#6379,#1554,.T.);
#8263=EDGE_CURVE('',#6391,#6512,#1555,.T.);
#8264=EDGE_CURVE('',#6512,#6513,#1104,.T.);
#8265=EDGE_CURVE('',#6514,#6513,#465,.T.);
#8266=EDGE_CURVE('',#6514,#6385,#1556,.T.);
#8267=EDGE_CURVE('',#6514,#6515,#1557,.T.);
#8268=EDGE_CURVE('',#6516,#6515,#1558,.T.);
#8269=EDGE_CURVE('',#6516,#6517,#1559,.T.);
#8270=EDGE_CURVE('',#6518,#6517,#1560,.T.);
#8271=EDGE_CURVE('',#6518,#6519,#1561,.T.);
#8272=EDGE_CURVE('',#6520,#6519,#1562,.T.);
#8273=EDGE_CURVE('',#6520,#6521,#1563,.T.);
#8274=EDGE_CURVE('',#6522,#6521,#1564,.T.);
#8275=EDGE_CURVE('',#6522,#6523,#1565,.T.);
#8276=EDGE_CURVE('',#6524,#6523,#1566,.T.);
#8277=EDGE_CURVE('',#6524,#6525,#1567,.T.);
#8278=EDGE_CURVE('',#6397,#6525,#1568,.T.);
#8279=EDGE_CURVE('',#6402,#6411,#1569,.T.);
#8280=EDGE_CURVE('',#6421,#6410,#1570,.T.);
#8281=EDGE_CURVE('',#6433,#6420,#1571,.T.);
#8282=EDGE_CURVE('',#6445,#6432,#1572,.T.);
#8283=EDGE_CURVE('',#6457,#6444,#1573,.T.);
#8284=EDGE_CURVE('',#6469,#6456,#1574,.T.);
#8285=EDGE_CURVE('',#6481,#6468,#1575,.T.);
#8286=EDGE_CURVE('',#6493,#6480,#1576,.T.);
#8287=EDGE_CURVE('',#6505,#6492,#1577,.T.);
#8288=EDGE_CURVE('',#6526,#6511,#1578,.T.);
#8289=EDGE_CURVE('',#6527,#6526,#1579,.T.);
#8290=EDGE_CURVE('',#6528,#6527,#1580,.T.);
#8291=EDGE_CURVE('',#6529,#6528,#1581,.T.);
#8292=EDGE_CURVE('',#6530,#6529,#1582,.T.);
#8293=EDGE_CURVE('',#6531,#6530,#1583,.T.);
#8294=EDGE_CURVE('',#6532,#6531,#1584,.T.);
#8295=EDGE_CURVE('',#6533,#6532,#1585,.T.);
#8296=EDGE_CURVE('',#6534,#6533,#1586,.T.);
#8297=EDGE_CURVE('',#6535,#6534,#1587,.T.);
#8298=EDGE_CURVE('',#6536,#6535,#1588,.T.);
#8299=EDGE_CURVE('',#6537,#6536,#1589,.T.);
#8300=EDGE_CURVE('',#6538,#6537,#1590,.T.);
#8301=EDGE_CURVE('',#6539,#6538,#1591,.T.);
#8302=EDGE_CURVE('',#6540,#6539,#1592,.T.);
#8303=EDGE_CURVE('',#6541,#6540,#1593,.T.);
#8304=EDGE_CURVE('',#6542,#6541,#1594,.T.);
#8305=EDGE_CURVE('',#6346,#6542,#1595,.T.);
#8306=EDGE_CURVE('',#6345,#6543,#1596,.T.);
#8307=EDGE_CURVE('',#6544,#6543,#1597,.T.);
#8308=EDGE_CURVE('',#6544,#6545,#1598,.T.);
#8309=EDGE_CURVE('',#6546,#6545,#1599,.T.);
#8310=EDGE_CURVE('',#6547,#6546,#1600,.T.);
#8311=EDGE_CURVE('',#6548,#6547,#1601,.T.);
#8312=EDGE_CURVE('',#6549,#6548,#1602,.T.);
#8313=EDGE_CURVE('',#6550,#6549,#1603,.T.);
#8314=EDGE_CURVE('',#6551,#6550,#1604,.T.);
#8315=EDGE_CURVE('',#6552,#6551,#1605,.T.);
#8316=EDGE_CURVE('',#6553,#6552,#1606,.T.);
#8317=EDGE_CURVE('',#6554,#6553,#1607,.T.);
#8318=EDGE_CURVE('',#6555,#6554,#1608,.T.);
#8319=EDGE_CURVE('',#6556,#6555,#1609,.T.);
#8320=EDGE_CURVE('',#6557,#6556,#1610,.T.);
#8321=EDGE_CURVE('',#6558,#6557,#1611,.T.);
#8322=EDGE_CURVE('',#6559,#6558,#1612,.T.);
#8323=EDGE_CURVE('',#6560,#6559,#1613,.T.);
#8324=EDGE_CURVE('',#6561,#6560,#1614,.T.);
#8325=EDGE_CURVE('',#6562,#6561,#1615,.T.);
#8326=EDGE_CURVE('',#6562,#6563,#1616,.T.);
#8327=EDGE_CURVE('',#6564,#6563,#1617,.T.);
#8328=EDGE_CURVE('',#6565,#6564,#1618,.T.);
#8329=EDGE_CURVE('',#6566,#6565,#1619,.T.);
#8330=EDGE_CURVE('',#6566,#6567,#1620,.T.);
#8331=EDGE_CURVE('',#6568,#6567,#1621,.T.);
#8332=EDGE_CURVE('',#6569,#6568,#1622,.T.);
#8333=EDGE_CURVE('',#6570,#6569,#1623,.T.);
#8334=EDGE_CURVE('',#6571,#6570,#1624,.T.);
#8335=EDGE_CURVE('',#6572,#6571,#1625,.T.);
#8336=EDGE_CURVE('',#6573,#6572,#1626,.T.);
#8337=EDGE_CURVE('',#6574,#6573,#1627,.T.);
#8338=EDGE_CURVE('',#6575,#6574,#1628,.T.);
#8339=EDGE_CURVE('',#6576,#6575,#1629,.T.);
#8340=EDGE_CURVE('',#6577,#6576,#1630,.T.);
#8341=EDGE_CURVE('',#6578,#6577,#1631,.T.);
#8342=EDGE_CURVE('',#6579,#6578,#1632,.T.);
#8343=EDGE_CURVE('',#6580,#6579,#1633,.T.);
#8344=EDGE_CURVE('',#6581,#6580,#1634,.T.);
#8345=EDGE_CURVE('',#6582,#6581,#1635,.T.);
#8346=EDGE_CURVE('',#6582,#6583,#1636,.T.);
#8347=EDGE_CURVE('',#6584,#6583,#1637,.T.);
#8348=EDGE_CURVE('',#6585,#6584,#1638,.T.);
#8349=EDGE_CURVE('',#6586,#6585,#1639,.T.);
#8350=EDGE_CURVE('',#6587,#6586,#1640,.T.);
#8351=EDGE_CURVE('',#6588,#6587,#1641,.T.);
#8352=EDGE_CURVE('',#6588,#6589,#1642,.T.);
#8353=EDGE_CURVE('',#6590,#6589,#1643,.T.);
#8354=EDGE_CURVE('',#6591,#6590,#1644,.T.);
#8355=EDGE_CURVE('',#6592,#6591,#1645,.T.);
#8356=EDGE_CURVE('',#6593,#6592,#1646,.T.);
#8357=EDGE_CURVE('',#6594,#6593,#1647,.T.);
#8358=EDGE_CURVE('',#6595,#6594,#1648,.T.);
#8359=EDGE_CURVE('',#6596,#6595,#1649,.T.);
#8360=EDGE_CURVE('',#6597,#6596,#1650,.T.);
#8361=EDGE_CURVE('',#6598,#6597,#1651,.T.);
#8362=EDGE_CURVE('',#6599,#6598,#1652,.T.);
#8363=EDGE_CURVE('',#6600,#6599,#1653,.T.);
#8364=EDGE_CURVE('',#6601,#6600,#1654,.T.);
#8365=EDGE_CURVE('',#6602,#6601,#1655,.T.);
#8366=EDGE_CURVE('',#6602,#6603,#1656,.T.);
#8367=EDGE_CURVE('',#6604,#6603,#1657,.T.);
#8368=EDGE_CURVE('',#6605,#6604,#1658,.T.);
#8369=EDGE_CURVE('',#6606,#6605,#1659,.T.);
#8370=EDGE_CURVE('',#6607,#6606,#1660,.T.);
#8371=EDGE_CURVE('',#6608,#6607,#1661,.T.);
#8372=EDGE_CURVE('',#6609,#6608,#1662,.T.);
#8373=EDGE_CURVE('',#6610,#6609,#1663,.T.);
#8374=EDGE_CURVE('',#6610,#6611,#1664,.T.);
#8375=EDGE_CURVE('',#6612,#6611,#1665,.T.);
#8376=EDGE_CURVE('',#6613,#6612,#1666,.T.);
#8377=EDGE_CURVE('',#6614,#6613,#1667,.T.);
#8378=EDGE_CURVE('',#6615,#6614,#1668,.T.);
#8379=EDGE_CURVE('',#6616,#6615,#1669,.T.);
#8380=EDGE_CURVE('',#6617,#6616,#1670,.T.);
#8381=EDGE_CURVE('',#6618,#6617,#1671,.T.);
#8382=EDGE_CURVE('',#6619,#6618,#1672,.T.);
#8383=EDGE_CURVE('',#6620,#6619,#1673,.T.);
#8384=EDGE_CURVE('',#6621,#6620,#1674,.T.);
#8385=EDGE_CURVE('',#6622,#6621,#1675,.T.);
#8386=EDGE_CURVE('',#6622,#6623,#1676,.T.);
#8387=EDGE_CURVE('',#6624,#6623,#1677,.T.);
#8388=EDGE_CURVE('',#6625,#6624,#1678,.T.);
#8389=EDGE_CURVE('',#6626,#6625,#1679,.T.);
#8390=EDGE_CURVE('',#6627,#6626,#1680,.T.);
#8391=EDGE_CURVE('',#6628,#6627,#1681,.T.);
#8392=EDGE_CURVE('',#6629,#6628,#1682,.T.);
#8393=EDGE_CURVE('',#6630,#6629,#1683,.T.);
#8394=EDGE_CURVE('',#6631,#6630,#1684,.T.);
#8395=EDGE_CURVE('',#6632,#6631,#1685,.T.);
#8396=EDGE_CURVE('',#6632,#6633,#1686,.T.);
#8397=EDGE_CURVE('',#6634,#6633,#1687,.T.);
#8398=EDGE_CURVE('',#6635,#6634,#1688,.T.);
#8399=EDGE_CURVE('',#6636,#6635,#1689,.T.);
#8400=EDGE_CURVE('',#6637,#6636,#1690,.T.);
#8401=EDGE_CURVE('',#6638,#6637,#1691,.T.);
#8402=EDGE_CURVE('',#6639,#6638,#1692,.T.);
#8403=EDGE_CURVE('',#6640,#6639,#1693,.T.);
#8404=EDGE_CURVE('',#6641,#6640,#1694,.T.);
#8405=EDGE_CURVE('',#6642,#6641,#1695,.T.);
#8406=EDGE_CURVE('',#6642,#6643,#1696,.T.);
#8407=EDGE_CURVE('',#6644,#6643,#1697,.T.);
#8408=EDGE_CURVE('',#6645,#6644,#1698,.T.);
#8409=EDGE_CURVE('',#6646,#6645,#1699,.T.);
#8410=EDGE_CURVE('',#6647,#6646,#1700,.T.);
#8411=EDGE_CURVE('',#6648,#6647,#1701,.T.);
#8412=EDGE_CURVE('',#6649,#6648,#1702,.T.);
#8413=EDGE_CURVE('',#6650,#6649,#1703,.T.);
#8414=EDGE_CURVE('',#6651,#6650,#1704,.T.);
#8415=EDGE_CURVE('',#6652,#6651,#1705,.T.);
#8416=EDGE_CURVE('',#6653,#6652,#1706,.T.);
#8417=EDGE_CURVE('',#6654,#6653,#1707,.T.);
#8418=EDGE_CURVE('',#6654,#6655,#1708,.T.);
#8419=EDGE_CURVE('',#6656,#6655,#1709,.T.);
#8420=EDGE_CURVE('',#6657,#6656,#1710,.T.);
#8421=EDGE_CURVE('',#6658,#6657,#1711,.T.);
#8422=EDGE_CURVE('',#6659,#6658,#1712,.T.);
#8423=EDGE_CURVE('',#6660,#6659,#1713,.T.);
#8424=EDGE_CURVE('',#6661,#6660,#1714,.T.);
#8425=EDGE_CURVE('',#6359,#6661,#1715,.T.);
#8426=EDGE_CURVE('',#6662,#6662,#1716,.T.);
#8427=EDGE_CURVE('',#6663,#6513,#4497,.T.);
#8428=EDGE_CURVE('',#6663,#6664,#1717,.T.);
#8429=EDGE_CURVE('',#6665,#6664,#4498,.T.);
#8430=EDGE_CURVE('',#6515,#6665,#466,.T.);
#8431=EDGE_CURVE('',#6512,#6666,#4499,.T.);
#8432=EDGE_CURVE('',#6666,#6663,#4500,.F.);
#8433=EDGE_CURVE('',#6667,#6668,#1105,.T.);
#8434=EDGE_CURVE('',#6668,#6669,#4501,.T.);
#8435=EDGE_CURVE('',#6669,#6670,#4502,.F.);
#8436=EDGE_CURVE('',#6670,#6671,#4503,.T.);
#8437=EDGE_CURVE('',#6671,#6667,#1106,.T.);
#8438=EDGE_CURVE('',#6671,#6672,#1718,.T.);
#8439=EDGE_CURVE('',#6673,#6672,#1107,.T.);
#8440=EDGE_CURVE('',#6673,#6657,#467,.T.);
#8441=EDGE_CURVE('',#6667,#6656,#468,.T.);
#8442=EDGE_CURVE('',#6670,#6674,#1719,.T.);
#8443=EDGE_CURVE('',#6672,#6674,#4504,.T.);
#8444=EDGE_CURVE('',#6675,#6674,#4505,.T.);
#8445=EDGE_CURVE('',#6675,#6676,#4506,.T.);
#8446=EDGE_CURVE('',#6676,#6673,#1108,.T.);
#8447=EDGE_CURVE('',#6677,#6678,#1109,.T.);
#8448=EDGE_CURVE('',#6678,#6679,#4507,.T.);
#8449=EDGE_CURVE('',#6679,#6680,#4508,.F.);
#8450=EDGE_CURVE('',#6680,#6681,#4509,.T.);
#8451=EDGE_CURVE('',#6681,#6677,#1110,.T.);
#8452=EDGE_CURVE('',#6681,#6682,#1720,.T.);
#8453=EDGE_CURVE('',#6683,#6682,#1111,.T.);
#8454=EDGE_CURVE('',#6683,#6659,#469,.T.);
#8455=EDGE_CURVE('',#6677,#6658,#470,.T.);
#8456=EDGE_CURVE('',#6680,#6684,#1721,.T.);
#8457=EDGE_CURVE('',#6682,#6684,#4510,.T.);
#8458=EDGE_CURVE('',#6685,#6684,#4511,.T.);
#8459=EDGE_CURVE('',#6685,#6686,#4512,.T.);
#8460=EDGE_CURVE('',#6686,#6683,#1112,.T.);
#8461=EDGE_CURVE('',#6687,#6688,#1113,.T.);
#8462=EDGE_CURVE('',#6688,#6689,#4513,.T.);
#8463=EDGE_CURVE('',#6689,#6690,#4514,.F.);
#8464=EDGE_CURVE('',#6690,#6691,#4515,.T.);
#8465=EDGE_CURVE('',#6691,#6687,#1114,.T.);
#8466=EDGE_CURVE('',#6691,#6692,#1722,.T.);
#8467=EDGE_CURVE('',#6693,#6692,#1115,.T.);
#8468=EDGE_CURVE('',#6693,#6661,#471,.T.);
#8469=EDGE_CURVE('',#6687,#6660,#472,.T.);
#8470=EDGE_CURVE('',#6690,#6694,#1723,.T.);
#8471=EDGE_CURVE('',#6692,#6694,#4516,.T.);
#8472=EDGE_CURVE('',#6360,#6695,#1116,.T.);
#8473=EDGE_CURVE('',#6695,#6696,#4517,.T.);
#8474=EDGE_CURVE('',#6696,#6361,#4518,.F.);
#8475=EDGE_CURVE('',#6697,#6695,#1724,.T.);
#8476=EDGE_CURVE('',#6698,#6697,#4519,.T.);
#8477=EDGE_CURVE('',#6696,#6698,#1725,.T.);
#8478=EDGE_CURVE('',#6697,#6693,#1117,.T.);
#8479=EDGE_CURVE('',#6698,#6694,#4520,.T.);
#8480=EDGE_CURVE('',#6699,#6700,#4521,.T.);
#8481=EDGE_CURVE('',#6699,#6701,#4522,.T.);
#8482=EDGE_CURVE('',#6701,#6702,#1118,.T.);
#8483=EDGE_CURVE('',#6702,#6700,#4523,.T.);
#8484=EDGE_CURVE('',#6701,#6703,#1726,.T.);
#8485=EDGE_CURVE('',#6704,#6703,#1119,.T.);
#8486=EDGE_CURVE('',#6704,#6644,#473,.T.);
#8487=EDGE_CURVE('',#6702,#6643,#474,.T.);
#8488=EDGE_CURVE('',#6705,#6699,#1727,.T.);
#8489=EDGE_CURVE('',#6703,#6705,#4524,.T.);
#8490=EDGE_CURVE('',#6705,#6706,#4525,.F.);
#8491=EDGE_CURVE('',#6706,#6707,#4526,.T.);
#8492=EDGE_CURVE('',#6707,#6704,#1120,.T.);
#8493=EDGE_CURVE('',#6708,#6709,#4527,.T.);
#8494=EDGE_CURVE('',#6708,#6710,#4528,.T.);
#8495=EDGE_CURVE('',#6710,#6711,#1121,.T.);
#8496=EDGE_CURVE('',#6711,#6712,#1122,.T.);
#8497=EDGE_CURVE('',#6712,#6709,#4529,.T.);
#8498=EDGE_CURVE('',#6710,#6713,#1728,.T.);
#8499=EDGE_CURVE('',#6714,#6713,#1123,.T.);
#8500=EDGE_CURVE('',#6714,#6646,#475,.T.);
#8501=EDGE_CURVE('',#6711,#6645,#476,.T.);
#8502=EDGE_CURVE('',#6715,#6708,#1729,.T.);
#8503=EDGE_CURVE('',#6713,#6715,#4530,.T.);
#8504=EDGE_CURVE('',#6715,#6716,#4531,.F.);
#8505=EDGE_CURVE('',#6716,#6717,#4532,.T.);
#8506=EDGE_CURVE('',#6717,#6714,#1124,.T.);
#8507=EDGE_CURVE('',#6718,#6719,#4533,.T.);
#8508=EDGE_CURVE('',#6718,#6720,#4534,.T.);
#8509=EDGE_CURVE('',#6720,#6721,#1125,.T.);
#8510=EDGE_CURVE('',#6721,#6722,#1126,.T.);
#8511=EDGE_CURVE('',#6722,#6719,#4535,.T.);
#8512=EDGE_CURVE('',#6720,#6723,#1730,.T.);
#8513=EDGE_CURVE('',#6724,#6723,#1127,.T.);
#8514=EDGE_CURVE('',#6724,#6648,#477,.T.);
#8515=EDGE_CURVE('',#6721,#6647,#478,.T.);
#8516=EDGE_CURVE('',#6725,#6718,#1731,.T.);
#8517=EDGE_CURVE('',#6723,#6725,#4536,.T.);
#8518=EDGE_CURVE('',#6725,#6726,#4537,.F.);
#8519=EDGE_CURVE('',#6726,#6727,#4538,.T.);
#8520=EDGE_CURVE('',#6727,#6724,#1128,.T.);
#8521=EDGE_CURVE('',#6728,#6729,#4539,.T.);
#8522=EDGE_CURVE('',#6728,#6730,#4540,.T.);
#8523=EDGE_CURVE('',#6730,#6731,#1129,.T.);
#8524=EDGE_CURVE('',#6731,#6732,#1130,.T.);
#8525=EDGE_CURVE('',#6732,#6729,#4541,.T.);
#8526=EDGE_CURVE('',#6730,#6733,#1732,.T.);
#8527=EDGE_CURVE('',#6734,#6733,#1131,.T.);
#8528=EDGE_CURVE('',#6734,#6650,#479,.T.);
#8529=EDGE_CURVE('',#6731,#6649,#480,.T.);
#8530=EDGE_CURVE('',#6735,#6728,#1733,.T.);
#8531=EDGE_CURVE('',#6733,#6735,#4542,.T.);
#8532=EDGE_CURVE('',#6735,#6736,#4543,.F.);
#8533=EDGE_CURVE('',#6736,#6737,#4544,.T.);
#8534=EDGE_CURVE('',#6737,#6734,#1132,.T.);
#8535=EDGE_CURVE('',#6738,#6739,#4545,.T.);
#8536=EDGE_CURVE('',#6738,#6740,#4546,.T.);
#8537=EDGE_CURVE('',#6740,#6741,#1133,.T.);
#8538=EDGE_CURVE('',#6741,#6742,#1134,.T.);
#8539=EDGE_CURVE('',#6742,#6739,#4547,.T.);
#8540=EDGE_CURVE('',#6740,#6743,#1734,.T.);
#8541=EDGE_CURVE('',#6744,#6743,#1135,.T.);
#8542=EDGE_CURVE('',#6744,#6652,#481,.T.);
#8543=EDGE_CURVE('',#6741,#6651,#482,.T.);
#8544=EDGE_CURVE('',#6745,#6738,#1735,.T.);
#8545=EDGE_CURVE('',#6743,#6745,#4548,.T.);
#8546=EDGE_CURVE('',#6745,#6746,#4549,.F.);
#8547=EDGE_CURVE('',#6746,#6747,#4550,.T.);
#8548=EDGE_CURVE('',#6747,#6744,#1136,.T.);
#8549=EDGE_CURVE('',#6748,#6749,#4551,.T.);
#8550=EDGE_CURVE('',#6748,#6750,#4552,.T.);
#8551=EDGE_CURVE('',#6750,#6751,#1137,.T.);
#8552=EDGE_CURVE('',#6751,#6752,#1138,.T.);
#8553=EDGE_CURVE('',#6752,#6749,#4553,.T.);
#8554=EDGE_CURVE('',#6750,#6753,#1736,.T.);
#8555=EDGE_CURVE('',#6754,#6753,#1139,.T.);
#8556=EDGE_CURVE('',#6654,#6754,#483,.T.);
#8557=EDGE_CURVE('',#6751,#6653,#484,.T.);
#8558=EDGE_CURVE('',#6755,#6748,#1737,.T.);
#8559=EDGE_CURVE('',#6753,#6755,#4554,.T.);
#8560=EDGE_CURVE('',#6756,#6757,#4555,.T.);
#8561=EDGE_CURVE('',#6758,#6757,#4556,.T.);
#8562=EDGE_CURVE('',#6758,#6759,#4557,.T.);
#8563=EDGE_CURVE('',#6759,#6756,#485,.T.);
#8564=EDGE_CURVE('',#6655,#6756,#486,.T.);
#8565=EDGE_CURVE('',#6759,#6668,#1738,.T.);
#8566=EDGE_CURVE('',#6676,#6678,#1739,.T.);
#8567=EDGE_CURVE('',#6686,#6688,#1740,.T.);
#8568=EDGE_CURVE('',#6689,#6685,#1741,.T.);
#8569=EDGE_CURVE('',#6679,#6675,#1742,.T.);
#8570=EDGE_CURVE('',#6669,#6758,#1743,.T.);
#8571=EDGE_CURVE('',#6755,#6760,#4558,.F.);
#8572=EDGE_CURVE('',#6760,#6754,#4559,.T.);
#8573=EDGE_CURVE('',#6707,#6712,#1744,.T.);
#8574=EDGE_CURVE('',#6717,#6722,#1745,.T.);
#8575=EDGE_CURVE('',#6727,#6732,#1746,.T.);
#8576=EDGE_CURVE('',#6737,#6742,#1747,.T.);
#8577=EDGE_CURVE('',#6747,#6752,#1748,.T.);
#8578=EDGE_CURVE('',#6760,#6757,#1749,.T.);
#8579=EDGE_CURVE('',#6746,#6749,#1750,.T.);
#8580=EDGE_CURVE('',#6736,#6739,#1751,.T.);
#8581=EDGE_CURVE('',#6726,#6729,#1752,.T.);
#8582=EDGE_CURVE('',#6716,#6719,#1753,.T.);
#8583=EDGE_CURVE('',#6706,#6709,#1754,.T.);
#8584=EDGE_CURVE('',#6761,#6762,#1140,.T.);
#8585=EDGE_CURVE('',#6762,#6763,#4560,.T.);
#8586=EDGE_CURVE('',#6763,#6764,#4561,.F.);
#8587=EDGE_CURVE('',#6764,#6765,#4562,.T.);
#8588=EDGE_CURVE('',#6765,#6761,#1141,.T.);
#8589=EDGE_CURVE('',#6765,#6766,#1755,.T.);
#8590=EDGE_CURVE('',#6767,#6766,#1142,.T.);
#8591=EDGE_CURVE('',#6635,#6767,#487,.T.);
#8592=EDGE_CURVE('',#6761,#6634,#488,.T.);
#8593=EDGE_CURVE('',#6764,#6768,#1756,.T.);
#8594=EDGE_CURVE('',#6766,#6768,#4563,.T.);
#8595=EDGE_CURVE('',#6769,#6768,#4564,.T.);
#8596=EDGE_CURVE('',#6769,#6770,#4565,.T.);
#8597=EDGE_CURVE('',#6770,#6767,#1143,.T.);
#8598=EDGE_CURVE('',#6770,#6771,#1757,.T.);
#8599=EDGE_CURVE('',#6772,#6771,#1144,.T.);
#8600=EDGE_CURVE('',#6772,#6636,#489,.T.);
#8601=EDGE_CURVE('',#6771,#6773,#4566,.T.);
#8602=EDGE_CURVE('',#6773,#6774,#4567,.F.);
#8603=EDGE_CURVE('',#6774,#6775,#4568,.T.);
#8604=EDGE_CURVE('',#6775,#6772,#1145,.T.);
#8605=EDGE_CURVE('',#6775,#6776,#1758,.T.);
#8606=EDGE_CURVE('',#6777,#6776,#1146,.T.);
#8607=EDGE_CURVE('',#6777,#6637,#490,.T.);
#8608=EDGE_CURVE('',#6774,#6778,#1759,.T.);
#8609=EDGE_CURVE('',#6776,#6778,#4569,.T.);
#8610=EDGE_CURVE('',#6779,#6778,#4570,.T.);
#8611=EDGE_CURVE('',#6779,#6780,#4571,.T.);
#8612=EDGE_CURVE('',#6780,#6777,#1147,.T.);
#8613=EDGE_CURVE('',#6781,#6782,#1148,.T.);
#8614=EDGE_CURVE('',#6782,#6783,#4572,.T.);
#8615=EDGE_CURVE('',#6783,#6784,#4573,.F.);
#8616=EDGE_CURVE('',#6784,#6785,#4574,.T.);
#8617=EDGE_CURVE('',#6785,#6781,#1149,.T.);
#8618=EDGE_CURVE('',#6785,#6786,#1760,.T.);
#8619=EDGE_CURVE('',#6787,#6786,#1150,.T.);
#8620=EDGE_CURVE('',#6787,#6639,#491,.T.);
#8621=EDGE_CURVE('',#6781,#6638,#492,.T.);
#8622=EDGE_CURVE('',#6784,#6788,#1761,.T.);
#8623=EDGE_CURVE('',#6786,#6788,#4575,.T.);
#8624=EDGE_CURVE('',#6789,#6788,#4576,.T.);
#8625=EDGE_CURVE('',#6789,#6790,#4577,.T.);
#8626=EDGE_CURVE('',#6790,#6787,#1151,.T.);
#8627=EDGE_CURVE('',#6791,#6792,#1152,.T.);
#8628=EDGE_CURVE('',#6792,#6793,#4578,.T.);
#8629=EDGE_CURVE('',#6793,#6794,#4579,.F.);
#8630=EDGE_CURVE('',#6794,#6795,#4580,.T.);
#8631=EDGE_CURVE('',#6795,#6791,#1153,.T.);
#8632=EDGE_CURVE('',#6795,#6796,#1762,.T.);
#8633=EDGE_CURVE('',#6797,#6796,#1154,.T.);
#8634=EDGE_CURVE('',#6797,#6641,#493,.T.);
#8635=EDGE_CURVE('',#6791,#6640,#494,.T.);
#8636=EDGE_CURVE('',#6794,#6798,#1763,.T.);
#8637=EDGE_CURVE('',#6796,#6798,#4581,.T.);
#8638=EDGE_CURVE('',#6799,#6800,#1155,.T.);
#8639=EDGE_CURVE('',#6800,#6801,#4582,.T.);
#8640=EDGE_CURVE('',#6801,#6802,#4583,.F.);
#8641=EDGE_CURVE('',#6802,#6799,#4584,.T.);
#8642=EDGE_CURVE('',#6803,#6800,#1764,.T.);
#8643=EDGE_CURVE('',#6804,#6803,#4585,.T.);
#8644=EDGE_CURVE('',#6801,#6804,#1765,.T.);
#8645=EDGE_CURVE('',#6642,#6799,#495,.T.);
#8646=EDGE_CURVE('',#6803,#6797,#1156,.T.);
#8647=EDGE_CURVE('',#6804,#6798,#4586,.T.);
#8648=EDGE_CURVE('',#6805,#6806,#4587,.T.);
#8649=EDGE_CURVE('',#6805,#6807,#4588,.T.);
#8650=EDGE_CURVE('',#6807,#6808,#1157,.T.);
#8651=EDGE_CURVE('',#6808,#6806,#4589,.T.);
#8652=EDGE_CURVE('',#6807,#6809,#1766,.T.);
#8653=EDGE_CURVE('',#6810,#6809,#1158,.T.);
#8654=EDGE_CURVE('',#6810,#6624,#496,.T.);
#8655=EDGE_CURVE('',#6808,#6623,#497,.T.);
#8656=EDGE_CURVE('',#6811,#6805,#1767,.T.);
#8657=EDGE_CURVE('',#6809,#6811,#4590,.T.);
#8658=EDGE_CURVE('',#6811,#6812,#4591,.F.);
#8659=EDGE_CURVE('',#6812,#6813,#4592,.T.);
#8660=EDGE_CURVE('',#6813,#6810,#1159,.T.);
#8661=EDGE_CURVE('',#6814,#6815,#4593,.T.);
#8662=EDGE_CURVE('',#6814,#6816,#4594,.T.);
#8663=EDGE_CURVE('',#6816,#6817,#1160,.T.);
#8664=EDGE_CURVE('',#6817,#6818,#1161,.T.);
#8665=EDGE_CURVE('',#6818,#6815,#4595,.T.);
#8666=EDGE_CURVE('',#6816,#6819,#1768,.T.);
#8667=EDGE_CURVE('',#6820,#6819,#1162,.T.);
#8668=EDGE_CURVE('',#6820,#6626,#498,.T.);
#8669=EDGE_CURVE('',#6817,#6625,#499,.T.);
#8670=EDGE_CURVE('',#6821,#6814,#1769,.T.);
#8671=EDGE_CURVE('',#6819,#6821,#4596,.T.);
#8672=EDGE_CURVE('',#6821,#6822,#4597,.F.);
#8673=EDGE_CURVE('',#6822,#6823,#4598,.T.);
#8674=EDGE_CURVE('',#6823,#6820,#1163,.T.);
#8675=EDGE_CURVE('',#6824,#6825,#4599,.T.);
#8676=EDGE_CURVE('',#6824,#6826,#4600,.T.);
#8677=EDGE_CURVE('',#6826,#6827,#1164,.T.);
#8678=EDGE_CURVE('',#6827,#6828,#1165,.T.);
#8679=EDGE_CURVE('',#6828,#6825,#4601,.T.);
#8680=EDGE_CURVE('',#6826,#6829,#1770,.T.);
#8681=EDGE_CURVE('',#6830,#6829,#1166,.T.);
#8682=EDGE_CURVE('',#6830,#6628,#500,.T.);
#8683=EDGE_CURVE('',#6827,#6627,#501,.T.);
#8684=EDGE_CURVE('',#6831,#6824,#1771,.T.);
#8685=EDGE_CURVE('',#6829,#6831,#4602,.T.);
#8686=EDGE_CURVE('',#6831,#6832,#4603,.F.);
#8687=EDGE_CURVE('',#6832,#6833,#4604,.T.);
#8688=EDGE_CURVE('',#6833,#6830,#1167,.T.);
#8689=EDGE_CURVE('',#6834,#6835,#4605,.T.);
#8690=EDGE_CURVE('',#6834,#6836,#4606,.T.);
#8691=EDGE_CURVE('',#6836,#6837,#1168,.T.);
#8692=EDGE_CURVE('',#6837,#6838,#1169,.T.);
#8693=EDGE_CURVE('',#6838,#6835,#4607,.T.);
#8694=EDGE_CURVE('',#6836,#6839,#1772,.T.);
#8695=EDGE_CURVE('',#6840,#6839,#1170,.T.);
#8696=EDGE_CURVE('',#6840,#6630,#502,.T.);
#8697=EDGE_CURVE('',#6837,#6629,#503,.T.);
#8698=EDGE_CURVE('',#6841,#6834,#1773,.T.);
#8699=EDGE_CURVE('',#6839,#6841,#4608,.T.);
#8700=EDGE_CURVE('',#6841,#6842,#4609,.F.);
#8701=EDGE_CURVE('',#6842,#6843,#4610,.T.);
#8702=EDGE_CURVE('',#6843,#6840,#1171,.T.);
#8703=EDGE_CURVE('',#6844,#6845,#4611,.T.);
#8704=EDGE_CURVE('',#6844,#6846,#4612,.T.);
#8705=EDGE_CURVE('',#6846,#6847,#1172,.T.);
#8706=EDGE_CURVE('',#6847,#6848,#1173,.T.);
#8707=EDGE_CURVE('',#6848,#6845,#4613,.T.);
#8708=EDGE_CURVE('',#6846,#6849,#1774,.T.);
#8709=EDGE_CURVE('',#6850,#6849,#1174,.T.);
#8710=EDGE_CURVE('',#6632,#6850,#504,.T.);
#8711=EDGE_CURVE('',#6631,#6847,#505,.T.);
#8712=EDGE_CURVE('',#6851,#6844,#1775,.T.);
#8713=EDGE_CURVE('',#6849,#6851,#4614,.T.);
#8714=EDGE_CURVE('',#6852,#6853,#4615,.T.);
#8715=EDGE_CURVE('',#6854,#6853,#4616,.T.);
#8716=EDGE_CURVE('',#6854,#6855,#4617,.T.);
#8717=EDGE_CURVE('',#6855,#6852,#506,.T.);
#8718=EDGE_CURVE('',#6633,#6852,#507,.T.);
#8719=EDGE_CURVE('',#6855,#6762,#1776,.T.);
#8720=EDGE_CURVE('',#6780,#6782,#1777,.T.);
#8721=EDGE_CURVE('',#6790,#6792,#1778,.T.);
#8722=EDGE_CURVE('',#6793,#6789,#1779,.T.);
#8723=EDGE_CURVE('',#6783,#6779,#1780,.T.);
#8724=EDGE_CURVE('',#6773,#6769,#1781,.T.);
#8725=EDGE_CURVE('',#6763,#6854,#1782,.T.);
#8726=EDGE_CURVE('',#6851,#6856,#4618,.F.);
#8727=EDGE_CURVE('',#6856,#6850,#4619,.T.);
#8728=EDGE_CURVE('',#6813,#6818,#1783,.T.);
#8729=EDGE_CURVE('',#6823,#6828,#1784,.T.);
#8730=EDGE_CURVE('',#6833,#6838,#1785,.T.);
#8731=EDGE_CURVE('',#6843,#6848,#1786,.T.);
#8732=EDGE_CURVE('',#6856,#6853,#1787,.T.);
#8733=EDGE_CURVE('',#6842,#6845,#1788,.T.);
#8734=EDGE_CURVE('',#6832,#6835,#1789,.T.);
#8735=EDGE_CURVE('',#6822,#6825,#1790,.T.);
#8736=EDGE_CURVE('',#6812,#6815,#1791,.T.);
#8737=EDGE_CURVE('',#6857,#6858,#1175,.T.);
#8738=EDGE_CURVE('',#6858,#6859,#4620,.T.);
#8739=EDGE_CURVE('',#6859,#6860,#4621,.F.);
#8740=EDGE_CURVE('',#6860,#6861,#4622,.T.);
#8741=EDGE_CURVE('',#6861,#6857,#1176,.T.);
#8742=EDGE_CURVE('',#6861,#6862,#1792,.T.);
#8743=EDGE_CURVE('',#6863,#6862,#1177,.T.);
#8744=EDGE_CURVE('',#6863,#6613,#508,.T.);
#8745=EDGE_CURVE('',#6857,#6612,#509,.T.);
#8746=EDGE_CURVE('',#6860,#6864,#1793,.T.);
#8747=EDGE_CURVE('',#6862,#6864,#4623,.T.);
#8748=EDGE_CURVE('',#6865,#6864,#4624,.T.);
#8749=EDGE_CURVE('',#6865,#6866,#4625,.T.);
#8750=EDGE_CURVE('',#6866,#6863,#1178,.T.);
#8751=EDGE_CURVE('',#6867,#6868,#1179,.T.);
#8752=EDGE_CURVE('',#6868,#6869,#4626,.T.);
#8753=EDGE_CURVE('',#6869,#6870,#4627,.F.);
#8754=EDGE_CURVE('',#6870,#6871,#4628,.T.);
#8755=EDGE_CURVE('',#6871,#6867,#1180,.T.);
#8756=EDGE_CURVE('',#6871,#6872,#1794,.T.);
#8757=EDGE_CURVE('',#6873,#6872,#1181,.T.);
#8758=EDGE_CURVE('',#6873,#6615,#510,.T.);
#8759=EDGE_CURVE('',#6867,#6614,#511,.T.);
#8760=EDGE_CURVE('',#6870,#6874,#1795,.T.);
#8761=EDGE_CURVE('',#6872,#6874,#4629,.T.);
#8762=EDGE_CURVE('',#6875,#6874,#4630,.T.);
#8763=EDGE_CURVE('',#6875,#6876,#4631,.T.);
#8764=EDGE_CURVE('',#6876,#6873,#1182,.T.);
#8765=EDGE_CURVE('',#6877,#6878,#1183,.T.);
#8766=EDGE_CURVE('',#6878,#6879,#4632,.T.);
#8767=EDGE_CURVE('',#6879,#6880,#4633,.F.);
#8768=EDGE_CURVE('',#6880,#6881,#4634,.T.);
#8769=EDGE_CURVE('',#6881,#6877,#1184,.T.);
#8770=EDGE_CURVE('',#6881,#6882,#1796,.T.);
#8771=EDGE_CURVE('',#6883,#6882,#1185,.T.);
#8772=EDGE_CURVE('',#6883,#6617,#512,.T.);
#8773=EDGE_CURVE('',#6877,#6616,#513,.T.);
#8774=EDGE_CURVE('',#6880,#6884,#1797,.T.);
#8775=EDGE_CURVE('',#6882,#6884,#4635,.T.);
#8776=EDGE_CURVE('',#6885,#6884,#4636,.T.);
#8777=EDGE_CURVE('',#6885,#6886,#4637,.T.);
#8778=EDGE_CURVE('',#6886,#6883,#1186,.T.);
#8779=EDGE_CURVE('',#6887,#6888,#1187,.T.);
#8780=EDGE_CURVE('',#6888,#6889,#4638,.T.);
#8781=EDGE_CURVE('',#6889,#6890,#4639,.F.);
#8782=EDGE_CURVE('',#6890,#6891,#4640,.T.);
#8783=EDGE_CURVE('',#6891,#6887,#1188,.T.);
#8784=EDGE_CURVE('',#6891,#6892,#1798,.T.);
#8785=EDGE_CURVE('',#6893,#6892,#1189,.T.);
#8786=EDGE_CURVE('',#6893,#6619,#514,.T.);
#8787=EDGE_CURVE('',#6887,#6618,#515,.T.);
#8788=EDGE_CURVE('',#6890,#6894,#1799,.T.);
#8789=EDGE_CURVE('',#6892,#6894,#4641,.T.);
#8790=EDGE_CURVE('',#6895,#6894,#4642,.T.);
#8791=EDGE_CURVE('',#6895,#6896,#4643,.T.);
#8792=EDGE_CURVE('',#6896,#6893,#1190,.T.);
#8793=EDGE_CURVE('',#6897,#6898,#1191,.T.);
#8794=EDGE_CURVE('',#6898,#6899,#4644,.T.);
#8795=EDGE_CURVE('',#6899,#6900,#4645,.F.);
#8796=EDGE_CURVE('',#6900,#6901,#4646,.T.);
#8797=EDGE_CURVE('',#6901,#6897,#1192,.T.);
#8798=EDGE_CURVE('',#6901,#6902,#1800,.T.);
#8799=EDGE_CURVE('',#6903,#6902,#1193,.T.);
#8800=EDGE_CURVE('',#6903,#6621,#516,.T.);
#8801=EDGE_CURVE('',#6897,#6620,#517,.T.);
#8802=EDGE_CURVE('',#6900,#6904,#1801,.T.);
#8803=EDGE_CURVE('',#6902,#6904,#4647,.T.);
#8804=EDGE_CURVE('',#6905,#6906,#1194,.T.);
#8805=EDGE_CURVE('',#6906,#6907,#4648,.T.);
#8806=EDGE_CURVE('',#6907,#6908,#4649,.F.);
#8807=EDGE_CURVE('',#6908,#6905,#4650,.T.);
#8808=EDGE_CURVE('',#6909,#6906,#1802,.T.);
#8809=EDGE_CURVE('',#6910,#6909,#4651,.T.);
#8810=EDGE_CURVE('',#6907,#6910,#1803,.T.);
#8811=EDGE_CURVE('',#6622,#6905,#518,.T.);
#8812=EDGE_CURVE('',#6909,#6903,#1195,.T.);
#8813=EDGE_CURVE('',#6910,#6904,#4652,.T.);
#8814=EDGE_CURVE('',#6911,#6912,#4653,.T.);
#8815=EDGE_CURVE('',#6911,#6913,#4654,.T.);
#8816=EDGE_CURVE('',#6913,#6914,#1196,.T.);
#8817=EDGE_CURVE('',#6914,#6912,#4655,.T.);
#8818=EDGE_CURVE('',#6913,#6915,#1804,.T.);
#8819=EDGE_CURVE('',#6916,#6915,#1197,.T.);
#8820=EDGE_CURVE('',#6916,#6604,#519,.T.);
#8821=EDGE_CURVE('',#6914,#6603,#520,.T.);
#8822=EDGE_CURVE('',#6917,#6911,#1805,.T.);
#8823=EDGE_CURVE('',#6915,#6917,#4656,.T.);
#8824=EDGE_CURVE('',#6917,#6918,#4657,.F.);
#8825=EDGE_CURVE('',#6918,#6919,#4658,.T.);
#8826=EDGE_CURVE('',#6919,#6916,#1198,.T.);
#8827=EDGE_CURVE('',#6920,#6921,#4659,.T.);
#8828=EDGE_CURVE('',#6920,#6922,#4660,.T.);
#8829=EDGE_CURVE('',#6922,#6923,#1199,.T.);
#8830=EDGE_CURVE('',#6923,#6924,#1200,.T.);
#8831=EDGE_CURVE('',#6924,#6921,#4661,.T.);
#8832=EDGE_CURVE('',#6922,#6925,#1806,.T.);
#8833=EDGE_CURVE('',#6926,#6925,#1201,.T.);
#8834=EDGE_CURVE('',#6926,#6606,#521,.T.);
#8835=EDGE_CURVE('',#6923,#6605,#522,.T.);
#8836=EDGE_CURVE('',#6927,#6920,#1807,.T.);
#8837=EDGE_CURVE('',#6925,#6927,#4662,.T.);
#8838=EDGE_CURVE('',#6927,#6928,#4663,.F.);
#8839=EDGE_CURVE('',#6928,#6929,#4664,.T.);
#8840=EDGE_CURVE('',#6929,#6926,#1202,.T.);
#8841=EDGE_CURVE('',#6930,#6931,#4665,.T.);
#8842=EDGE_CURVE('',#6930,#6932,#4666,.T.);
#8843=EDGE_CURVE('',#6932,#6933,#1203,.T.);
#8844=EDGE_CURVE('',#6933,#6934,#1204,.T.);
#8845=EDGE_CURVE('',#6934,#6931,#4667,.T.);
#8846=EDGE_CURVE('',#6932,#6935,#1808,.T.);
#8847=EDGE_CURVE('',#6936,#6935,#1205,.T.);
#8848=EDGE_CURVE('',#6936,#6608,#523,.T.);
#8849=EDGE_CURVE('',#6933,#6607,#524,.T.);
#8850=EDGE_CURVE('',#6937,#6930,#1809,.T.);
#8851=EDGE_CURVE('',#6935,#6937,#4668,.T.);
#8852=EDGE_CURVE('',#6937,#6938,#4669,.F.);
#8853=EDGE_CURVE('',#6938,#6939,#4670,.T.);
#8854=EDGE_CURVE('',#6939,#6936,#1206,.T.);
#8855=EDGE_CURVE('',#6940,#6941,#4671,.T.);
#8856=EDGE_CURVE('',#6940,#6942,#4672,.T.);
#8857=EDGE_CURVE('',#6942,#6943,#1207,.T.);
#8858=EDGE_CURVE('',#6943,#6944,#1208,.T.);
#8859=EDGE_CURVE('',#6944,#6941,#4673,.T.);
#8860=EDGE_CURVE('',#6942,#6945,#1810,.T.);
#8861=EDGE_CURVE('',#6946,#6945,#1209,.T.);
#8862=EDGE_CURVE('',#6610,#6946,#525,.T.);
#8863=EDGE_CURVE('',#6943,#6609,#526,.T.);
#8864=EDGE_CURVE('',#6947,#6940,#1811,.T.);
#8865=EDGE_CURVE('',#6945,#6947,#4674,.T.);
#8866=EDGE_CURVE('',#6948,#6949,#4675,.T.);
#8867=EDGE_CURVE('',#6950,#6949,#4676,.T.);
#8868=EDGE_CURVE('',#6950,#6951,#4677,.T.);
#8869=EDGE_CURVE('',#6951,#6948,#527,.T.);
#8870=EDGE_CURVE('',#6611,#6948,#528,.T.);
#8871=EDGE_CURVE('',#6951,#6858,#1812,.T.);
#8872=EDGE_CURVE('',#6866,#6868,#1813,.T.);
#8873=EDGE_CURVE('',#6876,#6878,#1814,.T.);
#8874=EDGE_CURVE('',#6886,#6888,#1815,.T.);
#8875=EDGE_CURVE('',#6896,#6898,#1816,.T.);
#8876=EDGE_CURVE('',#6899,#6895,#1817,.T.);
#8877=EDGE_CURVE('',#6889,#6885,#1818,.T.);
#8878=EDGE_CURVE('',#6879,#6875,#1819,.T.);
#8879=EDGE_CURVE('',#6869,#6865,#1820,.T.);
#8880=EDGE_CURVE('',#6859,#6950,#1821,.T.);
#8881=EDGE_CURVE('',#6947,#6952,#4678,.F.);
#8882=EDGE_CURVE('',#6952,#6946,#4679,.T.);
#8883=EDGE_CURVE('',#6919,#6924,#1822,.T.);
#8884=EDGE_CURVE('',#6929,#6934,#1823,.T.);
#8885=EDGE_CURVE('',#6939,#6944,#1824,.T.);
#8886=EDGE_CURVE('',#6952,#6949,#1825,.T.);
#8887=EDGE_CURVE('',#6938,#6941,#1826,.T.);
#8888=EDGE_CURVE('',#6928,#6931,#1827,.T.);
#8889=EDGE_CURVE('',#6918,#6921,#1828,.T.);
#8890=EDGE_CURVE('',#6953,#6954,#1210,.T.);
#8891=EDGE_CURVE('',#6954,#6955,#4680,.T.);
#8892=EDGE_CURVE('',#6955,#6956,#4681,.F.);
#8893=EDGE_CURVE('',#6956,#6957,#4682,.T.);
#8894=EDGE_CURVE('',#6957,#6953,#1211,.T.);
#8895=EDGE_CURVE('',#6957,#6958,#1829,.T.);
#8896=EDGE_CURVE('',#6959,#6958,#1212,.T.);
#8897=EDGE_CURVE('',#6591,#6959,#529,.T.);
#8898=EDGE_CURVE('',#6953,#6590,#530,.T.);
#8899=EDGE_CURVE('',#6956,#6960,#1830,.T.);
#8900=EDGE_CURVE('',#6958,#6960,#4683,.T.);
#8901=EDGE_CURVE('',#6961,#6960,#4684,.T.);
#8902=EDGE_CURVE('',#6961,#6962,#4685,.T.);
#8903=EDGE_CURVE('',#6962,#6959,#1213,.T.);
#8904=EDGE_CURVE('',#6962,#6963,#1831,.T.);
#8905=EDGE_CURVE('',#6964,#6963,#1214,.T.);
#8906=EDGE_CURVE('',#6964,#6592,#531,.T.);
#8907=EDGE_CURVE('',#6963,#6965,#4686,.T.);
#8908=EDGE_CURVE('',#6965,#6966,#4687,.F.);
#8909=EDGE_CURVE('',#6966,#6967,#4688,.T.);
#8910=EDGE_CURVE('',#6967,#6964,#1215,.T.);
#8911=EDGE_CURVE('',#6967,#6968,#1832,.T.);
#8912=EDGE_CURVE('',#6969,#6968,#1216,.T.);
#8913=EDGE_CURVE('',#6969,#6593,#532,.T.);
#8914=EDGE_CURVE('',#6966,#6970,#1833,.T.);
#8915=EDGE_CURVE('',#6968,#6970,#4689,.T.);
#8916=EDGE_CURVE('',#6971,#6970,#4690,.T.);
#8917=EDGE_CURVE('',#6971,#6972,#4691,.T.);
#8918=EDGE_CURVE('',#6972,#6969,#1217,.T.);
#8919=EDGE_CURVE('',#6973,#6974,#1218,.T.);
#8920=EDGE_CURVE('',#6974,#6975,#4692,.T.);
#8921=EDGE_CURVE('',#6975,#6976,#4693,.F.);
#8922=EDGE_CURVE('',#6976,#6977,#4694,.T.);
#8923=EDGE_CURVE('',#6977,#6973,#1219,.T.);
#8924=EDGE_CURVE('',#6977,#6978,#1834,.T.);
#8925=EDGE_CURVE('',#6979,#6978,#1220,.T.);
#8926=EDGE_CURVE('',#6979,#6595,#533,.T.);
#8927=EDGE_CURVE('',#6973,#6594,#534,.T.);
#8928=EDGE_CURVE('',#6976,#6980,#1835,.T.);
#8929=EDGE_CURVE('',#6978,#6980,#4695,.T.);
#8930=EDGE_CURVE('',#6981,#6980,#4696,.T.);
#8931=EDGE_CURVE('',#6981,#6982,#4697,.T.);
#8932=EDGE_CURVE('',#6982,#6979,#1221,.T.);
#8933=EDGE_CURVE('',#6983,#6984,#1222,.T.);
#8934=EDGE_CURVE('',#6984,#6985,#4698,.T.);
#8935=EDGE_CURVE('',#6985,#6986,#4699,.F.);
#8936=EDGE_CURVE('',#6986,#6987,#4700,.T.);
#8937=EDGE_CURVE('',#6987,#6983,#1223,.T.);
#8938=EDGE_CURVE('',#6987,#6988,#1836,.T.);
#8939=EDGE_CURVE('',#6989,#6988,#1224,.T.);
#8940=EDGE_CURVE('',#6989,#6597,#535,.T.);
#8941=EDGE_CURVE('',#6983,#6596,#536,.T.);
#8942=EDGE_CURVE('',#6986,#6990,#1837,.T.);
#8943=EDGE_CURVE('',#6988,#6990,#4701,.T.);
#8944=EDGE_CURVE('',#6991,#6990,#4702,.T.);
#8945=EDGE_CURVE('',#6991,#6992,#4703,.T.);
#8946=EDGE_CURVE('',#6992,#6989,#1225,.T.);
#8947=EDGE_CURVE('',#6993,#6994,#1226,.T.);
#8948=EDGE_CURVE('',#6994,#6995,#4704,.T.);
#8949=EDGE_CURVE('',#6995,#6996,#4705,.F.);
#8950=EDGE_CURVE('',#6996,#6997,#4706,.T.);
#8951=EDGE_CURVE('',#6997,#6993,#1227,.T.);
#8952=EDGE_CURVE('',#6997,#6998,#1838,.T.);
#8953=EDGE_CURVE('',#6999,#6998,#1228,.T.);
#8954=EDGE_CURVE('',#6999,#6599,#537,.T.);
#8955=EDGE_CURVE('',#6993,#6598,#538,.T.);
#8956=EDGE_CURVE('',#6996,#7000,#1839,.T.);
#8957=EDGE_CURVE('',#6998,#7000,#4707,.T.);
#8958=EDGE_CURVE('',#7001,#7000,#4708,.T.);
#8959=EDGE_CURVE('',#7001,#7002,#4709,.T.);
#8960=EDGE_CURVE('',#7002,#6999,#1229,.T.);
#8961=EDGE_CURVE('',#7003,#7004,#1230,.T.);
#8962=EDGE_CURVE('',#7004,#7005,#4710,.T.);
#8963=EDGE_CURVE('',#7005,#7006,#4711,.F.);
#8964=EDGE_CURVE('',#7006,#7007,#4712,.T.);
#8965=EDGE_CURVE('',#7007,#7003,#1231,.T.);
#8966=EDGE_CURVE('',#7007,#7008,#1840,.T.);
#8967=EDGE_CURVE('',#7009,#7008,#1232,.T.);
#8968=EDGE_CURVE('',#7009,#6601,#539,.T.);
#8969=EDGE_CURVE('',#7003,#6600,#540,.T.);
#8970=EDGE_CURVE('',#7006,#7010,#1841,.T.);
#8971=EDGE_CURVE('',#7008,#7010,#4713,.T.);
#8972=EDGE_CURVE('',#7011,#7012,#1233,.T.);
#8973=EDGE_CURVE('',#7012,#7013,#4714,.T.);
#8974=EDGE_CURVE('',#7013,#7014,#4715,.F.);
#8975=EDGE_CURVE('',#7014,#7011,#4716,.T.);
#8976=EDGE_CURVE('',#7015,#7012,#1842,.T.);
#8977=EDGE_CURVE('',#7016,#7015,#4717,.T.);
#8978=EDGE_CURVE('',#7013,#7016,#1843,.T.);
#8979=EDGE_CURVE('',#6602,#7011,#541,.T.);
#8980=EDGE_CURVE('',#7015,#7009,#1234,.T.);
#8981=EDGE_CURVE('',#7016,#7010,#4718,.T.);
#8982=EDGE_CURVE('',#7017,#7018,#4719,.T.);
#8983=EDGE_CURVE('',#7017,#7019,#4720,.T.);
#8984=EDGE_CURVE('',#7019,#7020,#1235,.T.);
#8985=EDGE_CURVE('',#7020,#7018,#4721,.T.);
#8986=EDGE_CURVE('',#7019,#7021,#1844,.T.);
#8987=EDGE_CURVE('',#7022,#7021,#1236,.T.);
#8988=EDGE_CURVE('',#7022,#6584,#542,.T.);
#8989=EDGE_CURVE('',#7020,#6583,#543,.T.);
#8990=EDGE_CURVE('',#7023,#7017,#1845,.T.);
#8991=EDGE_CURVE('',#7021,#7023,#4722,.T.);
#8992=EDGE_CURVE('',#7023,#7024,#4723,.F.);
#8993=EDGE_CURVE('',#7024,#7025,#4724,.T.);
#8994=EDGE_CURVE('',#7025,#7022,#1237,.T.);
#8995=EDGE_CURVE('',#7026,#7027,#4725,.T.);
#8996=EDGE_CURVE('',#7026,#7028,#4726,.T.);
#8997=EDGE_CURVE('',#7028,#7029,#1238,.T.);
#8998=EDGE_CURVE('',#7029,#7030,#1239,.T.);
#8999=EDGE_CURVE('',#7030,#7027,#4727,.T.);
#9000=EDGE_CURVE('',#7028,#7031,#1846,.T.);
#9001=EDGE_CURVE('',#7032,#7031,#1240,.T.);
#9002=EDGE_CURVE('',#7032,#6586,#544,.T.);
#9003=EDGE_CURVE('',#7029,#6585,#545,.T.);
#9004=EDGE_CURVE('',#7033,#7026,#1847,.T.);
#9005=EDGE_CURVE('',#7031,#7033,#4728,.T.);
#9006=EDGE_CURVE('',#7033,#7034,#4729,.F.);
#9007=EDGE_CURVE('',#7034,#7035,#4730,.T.);
#9008=EDGE_CURVE('',#7035,#7032,#1241,.T.);
#9009=EDGE_CURVE('',#7036,#7037,#4731,.T.);
#9010=EDGE_CURVE('',#7036,#7038,#4732,.T.);
#9011=EDGE_CURVE('',#7038,#7039,#1242,.T.);
#9012=EDGE_CURVE('',#7039,#7040,#1243,.T.);
#9013=EDGE_CURVE('',#7040,#7037,#4733,.T.);
#9014=EDGE_CURVE('',#7038,#7041,#1848,.T.);
#9015=EDGE_CURVE('',#7042,#7041,#1244,.T.);
#9016=EDGE_CURVE('',#6588,#7042,#546,.T.);
#9017=EDGE_CURVE('',#6587,#7039,#547,.T.);
#9018=EDGE_CURVE('',#7043,#7036,#1849,.T.);
#9019=EDGE_CURVE('',#7041,#7043,#4734,.T.);
#9020=EDGE_CURVE('',#7044,#7045,#4735,.T.);
#9021=EDGE_CURVE('',#7046,#7045,#4736,.T.);
#9022=EDGE_CURVE('',#7046,#7047,#4737,.T.);
#9023=EDGE_CURVE('',#7047,#7044,#548,.T.);
#9024=EDGE_CURVE('',#6589,#7044,#549,.T.);
#9025=EDGE_CURVE('',#7047,#6954,#1850,.T.);
#9026=EDGE_CURVE('',#6972,#6974,#1851,.T.);
#9027=EDGE_CURVE('',#6982,#6984,#1852,.T.);
#9028=EDGE_CURVE('',#6992,#6994,#1853,.T.);
#9029=EDGE_CURVE('',#7002,#7004,#1854,.T.);
#9030=EDGE_CURVE('',#7005,#7001,#1855,.T.);
#9031=EDGE_CURVE('',#6995,#6991,#1856,.T.);
#9032=EDGE_CURVE('',#6985,#6981,#1857,.T.);
#9033=EDGE_CURVE('',#6975,#6971,#1858,.T.);
#9034=EDGE_CURVE('',#6965,#6961,#1859,.T.);
#9035=EDGE_CURVE('',#6955,#7046,#1860,.T.);
#9036=EDGE_CURVE('',#7043,#7048,#4738,.F.);
#9037=EDGE_CURVE('',#7048,#7042,#4739,.T.);
#9038=EDGE_CURVE('',#7025,#7030,#1861,.T.);
#9039=EDGE_CURVE('',#7035,#7040,#1862,.T.);
#9040=EDGE_CURVE('',#7048,#7045,#1863,.T.);
#9041=EDGE_CURVE('',#7034,#7037,#1864,.T.);
#9042=EDGE_CURVE('',#7024,#7027,#1865,.T.);
#9043=EDGE_CURVE('',#7049,#7050,#1245,.T.);
#9044=EDGE_CURVE('',#7050,#7051,#4740,.T.);
#9045=EDGE_CURVE('',#7051,#7052,#4741,.F.);
#9046=EDGE_CURVE('',#7052,#7053,#4742,.T.);
#9047=EDGE_CURVE('',#7053,#7049,#1246,.T.);
#9048=EDGE_CURVE('',#7053,#7054,#1866,.T.);
#9049=EDGE_CURVE('',#7055,#7054,#1247,.T.);
#9050=EDGE_CURVE('',#7055,#6569,#550,.T.);
#9051=EDGE_CURVE('',#7049,#6568,#551,.T.);
#9052=EDGE_CURVE('',#7052,#7056,#1867,.T.);
#9053=EDGE_CURVE('',#7054,#7056,#4743,.T.);
#9054=EDGE_CURVE('',#7057,#7056,#4744,.T.);
#9055=EDGE_CURVE('',#7057,#7058,#4745,.T.);
#9056=EDGE_CURVE('',#7058,#7055,#1248,.T.);
#9057=EDGE_CURVE('',#7059,#7060,#1249,.T.);
#9058=EDGE_CURVE('',#7060,#7061,#4746,.T.);
#9059=EDGE_CURVE('',#7061,#7062,#4747,.F.);
#9060=EDGE_CURVE('',#7062,#7063,#4748,.T.);
#9061=EDGE_CURVE('',#7063,#7059,#1250,.T.);
#9062=EDGE_CURVE('',#7063,#7064,#1868,.T.);
#9063=EDGE_CURVE('',#7065,#7064,#1251,.T.);
#9064=EDGE_CURVE('',#7065,#6571,#552,.T.);
#9065=EDGE_CURVE('',#7059,#6570,#553,.T.);
#9066=EDGE_CURVE('',#7062,#7066,#1869,.T.);
#9067=EDGE_CURVE('',#7064,#7066,#4749,.T.);
#9068=EDGE_CURVE('',#7067,#7066,#4750,.T.);
#9069=EDGE_CURVE('',#7067,#7068,#4751,.T.);
#9070=EDGE_CURVE('',#7068,#7065,#1252,.T.);
#9071=EDGE_CURVE('',#7069,#7070,#1253,.T.);
#9072=EDGE_CURVE('',#7070,#7071,#4752,.T.);
#9073=EDGE_CURVE('',#7071,#7072,#4753,.F.);
#9074=EDGE_CURVE('',#7072,#7073,#4754,.T.);
#9075=EDGE_CURVE('',#7073,#7069,#1254,.T.);
#9076=EDGE_CURVE('',#7073,#7074,#1870,.T.);
#9077=EDGE_CURVE('',#7075,#7074,#1255,.T.);
#9078=EDGE_CURVE('',#7075,#6573,#554,.T.);
#9079=EDGE_CURVE('',#7069,#6572,#555,.T.);
#9080=EDGE_CURVE('',#7072,#7076,#1871,.T.);
#9081=EDGE_CURVE('',#7074,#7076,#4755,.T.);
#9082=EDGE_CURVE('',#7077,#7076,#4756,.T.);
#9083=EDGE_CURVE('',#7077,#7078,#4757,.T.);
#9084=EDGE_CURVE('',#7078,#7075,#1256,.T.);
#9085=EDGE_CURVE('',#7079,#7080,#1257,.T.);
#9086=EDGE_CURVE('',#7080,#7081,#4758,.T.);
#9087=EDGE_CURVE('',#7081,#7082,#4759,.F.);
#9088=EDGE_CURVE('',#7082,#7083,#4760,.T.);
#9089=EDGE_CURVE('',#7083,#7079,#1258,.T.);
#9090=EDGE_CURVE('',#7083,#7084,#1872,.T.);
#9091=EDGE_CURVE('',#7085,#7084,#1259,.T.);
#9092=EDGE_CURVE('',#7085,#6575,#556,.T.);
#9093=EDGE_CURVE('',#7079,#6574,#557,.T.);
#9094=EDGE_CURVE('',#7082,#7086,#1873,.T.);
#9095=EDGE_CURVE('',#7084,#7086,#4761,.T.);
#9096=EDGE_CURVE('',#7087,#7086,#4762,.T.);
#9097=EDGE_CURVE('',#7087,#7088,#4763,.T.);
#9098=EDGE_CURVE('',#7088,#7085,#1260,.T.);
#9099=EDGE_CURVE('',#7089,#7090,#1261,.T.);
#9100=EDGE_CURVE('',#7090,#7091,#4764,.T.);
#9101=EDGE_CURVE('',#7091,#7092,#4765,.F.);
#9102=EDGE_CURVE('',#7092,#7093,#4766,.T.);
#9103=EDGE_CURVE('',#7093,#7089,#1262,.T.);
#9104=EDGE_CURVE('',#7093,#7094,#1874,.T.);
#9105=EDGE_CURVE('',#7095,#7094,#1263,.T.);
#9106=EDGE_CURVE('',#7095,#6577,#558,.T.);
#9107=EDGE_CURVE('',#7089,#6576,#559,.T.);
#9108=EDGE_CURVE('',#7092,#7096,#1875,.T.);
#9109=EDGE_CURVE('',#7094,#7096,#4767,.T.);
#9110=EDGE_CURVE('',#7097,#7096,#4768,.T.);
#9111=EDGE_CURVE('',#7097,#7098,#4769,.T.);
#9112=EDGE_CURVE('',#7098,#7095,#1264,.T.);
#9113=EDGE_CURVE('',#7099,#7100,#1265,.T.);
#9114=EDGE_CURVE('',#7100,#7101,#4770,.T.);
#9115=EDGE_CURVE('',#7101,#7102,#4771,.F.);
#9116=EDGE_CURVE('',#7102,#7103,#4772,.T.);
#9117=EDGE_CURVE('',#7103,#7099,#1266,.T.);
#9118=EDGE_CURVE('',#7103,#7104,#1876,.T.);
#9119=EDGE_CURVE('',#7105,#7104,#1267,.T.);
#9120=EDGE_CURVE('',#7105,#6579,#560,.T.);
#9121=EDGE_CURVE('',#7099,#6578,#561,.T.);
#9122=EDGE_CURVE('',#7102,#7106,#1877,.T.);
#9123=EDGE_CURVE('',#7104,#7106,#4773,.T.);
#9124=EDGE_CURVE('',#7107,#7106,#4774,.T.);
#9125=EDGE_CURVE('',#7107,#7108,#4775,.T.);
#9126=EDGE_CURVE('',#7108,#7105,#1268,.T.);
#9127=EDGE_CURVE('',#7109,#7110,#1269,.T.);
#9128=EDGE_CURVE('',#7110,#7111,#4776,.T.);
#9129=EDGE_CURVE('',#7111,#7112,#4777,.F.);
#9130=EDGE_CURVE('',#7112,#7113,#4778,.T.);
#9131=EDGE_CURVE('',#7113,#7109,#1270,.T.);
#9132=EDGE_CURVE('',#7113,#7114,#1878,.T.);
#9133=EDGE_CURVE('',#7115,#7114,#1271,.T.);
#9134=EDGE_CURVE('',#7115,#6581,#562,.T.);
#9135=EDGE_CURVE('',#7109,#6580,#563,.T.);
#9136=EDGE_CURVE('',#7112,#7116,#1879,.T.);
#9137=EDGE_CURVE('',#7114,#7116,#4779,.T.);
#9138=EDGE_CURVE('',#7117,#7118,#1272,.T.);
#9139=EDGE_CURVE('',#7118,#7119,#4780,.T.);
#9140=EDGE_CURVE('',#7119,#7120,#4781,.F.);
#9141=EDGE_CURVE('',#7120,#7117,#4782,.T.);
#9142=EDGE_CURVE('',#7121,#7118,#1880,.T.);
#9143=EDGE_CURVE('',#7122,#7121,#4783,.T.);
#9144=EDGE_CURVE('',#7119,#7122,#1881,.T.);
#9145=EDGE_CURVE('',#6582,#7117,#564,.T.);
#9146=EDGE_CURVE('',#7121,#7115,#1273,.T.);
#9147=EDGE_CURVE('',#7122,#7116,#4784,.T.);
#9148=EDGE_CURVE('',#7123,#7124,#4785,.T.);
#9149=EDGE_CURVE('',#7123,#7125,#4786,.T.);
#9150=EDGE_CURVE('',#7125,#7126,#1274,.T.);
#9151=EDGE_CURVE('',#7126,#7124,#4787,.T.);
#9152=EDGE_CURVE('',#7125,#7127,#1882,.T.);
#9153=EDGE_CURVE('',#7128,#7127,#1275,.T.);
#9154=EDGE_CURVE('',#7128,#6564,#565,.T.);
#9155=EDGE_CURVE('',#7126,#6563,#566,.T.);
#9156=EDGE_CURVE('',#7129,#7123,#1883,.T.);
#9157=EDGE_CURVE('',#7127,#7129,#4788,.T.);
#9158=EDGE_CURVE('',#7129,#7130,#4789,.F.);
#9159=EDGE_CURVE('',#7130,#7131,#4790,.T.);
#9160=EDGE_CURVE('',#7131,#7128,#1276,.T.);
#9161=EDGE_CURVE('',#7132,#7133,#4791,.T.);
#9162=EDGE_CURVE('',#7132,#7134,#4792,.T.);
#9163=EDGE_CURVE('',#7134,#7135,#1277,.T.);
#9164=EDGE_CURVE('',#7135,#7136,#1278,.T.);
#9165=EDGE_CURVE('',#7136,#7133,#4793,.T.);
#9166=EDGE_CURVE('',#7134,#7137,#1884,.T.);
#9167=EDGE_CURVE('',#7138,#7137,#1279,.T.);
#9168=EDGE_CURVE('',#6566,#7138,#567,.T.);
#9169=EDGE_CURVE('',#7135,#6565,#568,.T.);
#9170=EDGE_CURVE('',#7139,#7132,#1885,.T.);
#9171=EDGE_CURVE('',#7137,#7139,#4794,.T.);
#9172=EDGE_CURVE('',#7140,#7141,#4795,.T.);
#9173=EDGE_CURVE('',#7142,#7141,#4796,.T.);
#9174=EDGE_CURVE('',#7142,#7143,#4797,.T.);
#9175=EDGE_CURVE('',#7143,#7140,#569,.T.);
#9176=EDGE_CURVE('',#6567,#7140,#570,.T.);
#9177=EDGE_CURVE('',#7143,#7050,#1886,.T.);
#9178=EDGE_CURVE('',#7058,#7060,#1887,.T.);
#9179=EDGE_CURVE('',#7068,#7070,#1888,.T.);
#9180=EDGE_CURVE('',#7078,#7080,#1889,.T.);
#9181=EDGE_CURVE('',#7088,#7090,#1890,.T.);
#9182=EDGE_CURVE('',#7098,#7100,#1891,.T.);
#9183=EDGE_CURVE('',#7108,#7110,#1892,.T.);
#9184=EDGE_CURVE('',#7111,#7107,#1893,.T.);
#9185=EDGE_CURVE('',#7101,#7097,#1894,.T.);
#9186=EDGE_CURVE('',#7091,#7087,#1895,.T.);
#9187=EDGE_CURVE('',#7081,#7077,#1896,.T.);
#9188=EDGE_CURVE('',#7071,#7067,#1897,.T.);
#9189=EDGE_CURVE('',#7061,#7057,#1898,.T.);
#9190=EDGE_CURVE('',#7051,#7142,#1899,.T.);
#9191=EDGE_CURVE('',#7139,#7144,#4798,.F.);
#9192=EDGE_CURVE('',#7144,#7138,#4799,.T.);
#9193=EDGE_CURVE('',#7131,#7136,#1900,.T.);
#9194=EDGE_CURVE('',#7144,#7141,#1901,.T.);
#9195=EDGE_CURVE('',#7130,#7133,#1902,.T.);
#9196=EDGE_CURVE('',#7145,#7146,#1280,.T.);
#9197=EDGE_CURVE('',#7146,#7147,#4800,.T.);
#9198=EDGE_CURVE('',#7147,#7148,#4801,.F.);
#9199=EDGE_CURVE('',#7148,#7149,#4802,.T.);
#9200=EDGE_CURVE('',#7149,#7145,#1281,.T.);
#9201=EDGE_CURVE('',#7149,#7150,#1903,.T.);
#9202=EDGE_CURVE('',#7151,#7150,#1282,.T.);
#9203=EDGE_CURVE('',#7151,#6547,#571,.T.);
#9204=EDGE_CURVE('',#7145,#6546,#572,.T.);
#9205=EDGE_CURVE('',#7148,#7152,#1904,.T.);
#9206=EDGE_CURVE('',#7150,#7152,#4803,.T.);
#9207=EDGE_CURVE('',#7153,#7152,#4804,.T.);
#9208=EDGE_CURVE('',#7153,#7154,#4805,.T.);
#9209=EDGE_CURVE('',#7154,#7151,#1283,.T.);
#9210=EDGE_CURVE('',#7155,#7156,#1284,.T.);
#9211=EDGE_CURVE('',#7156,#7157,#4806,.T.);
#9212=EDGE_CURVE('',#7157,#7158,#4807,.F.);
#9213=EDGE_CURVE('',#7158,#7159,#4808,.T.);
#9214=EDGE_CURVE('',#7159,#7155,#1285,.T.);
#9215=EDGE_CURVE('',#7159,#7160,#1905,.T.);
#9216=EDGE_CURVE('',#7161,#7160,#1286,.T.);
#9217=EDGE_CURVE('',#7161,#6549,#573,.T.);
#9218=EDGE_CURVE('',#7155,#6548,#574,.T.);
#9219=EDGE_CURVE('',#7158,#7162,#1906,.T.);
#9220=EDGE_CURVE('',#7160,#7162,#4809,.T.);
#9221=EDGE_CURVE('',#7163,#7162,#4810,.T.);
#9222=EDGE_CURVE('',#7163,#7164,#4811,.T.);
#9223=EDGE_CURVE('',#7164,#7161,#1287,.T.);
#9224=EDGE_CURVE('',#7165,#7166,#1288,.T.);
#9225=EDGE_CURVE('',#7166,#7167,#4812,.T.);
#9226=EDGE_CURVE('',#7167,#7168,#4813,.F.);
#9227=EDGE_CURVE('',#7168,#7169,#4814,.T.);
#9228=EDGE_CURVE('',#7169,#7165,#1289,.T.);
#9229=EDGE_CURVE('',#7169,#7170,#1907,.T.);
#9230=EDGE_CURVE('',#7171,#7170,#1290,.T.);
#9231=EDGE_CURVE('',#7171,#6551,#575,.T.);
#9232=EDGE_CURVE('',#7165,#6550,#576,.T.);
#9233=EDGE_CURVE('',#7168,#7172,#1908,.T.);
#9234=EDGE_CURVE('',#7170,#7172,#4815,.T.);
#9235=EDGE_CURVE('',#7173,#7172,#4816,.T.);
#9236=EDGE_CURVE('',#7173,#7174,#4817,.T.);
#9237=EDGE_CURVE('',#7174,#7171,#1291,.T.);
#9238=EDGE_CURVE('',#7175,#7176,#1292,.T.);
#9239=EDGE_CURVE('',#7176,#7177,#4818,.T.);
#9240=EDGE_CURVE('',#7177,#7178,#4819,.F.);
#9241=EDGE_CURVE('',#7178,#7179,#4820,.T.);
#9242=EDGE_CURVE('',#7179,#7175,#1293,.T.);
#9243=EDGE_CURVE('',#7179,#7180,#1909,.T.);
#9244=EDGE_CURVE('',#7181,#7180,#1294,.T.);
#9245=EDGE_CURVE('',#7181,#6553,#577,.T.);
#9246=EDGE_CURVE('',#7175,#6552,#578,.T.);
#9247=EDGE_CURVE('',#7178,#7182,#1910,.T.);
#9248=EDGE_CURVE('',#7180,#7182,#4821,.T.);
#9249=EDGE_CURVE('',#7183,#7182,#4822,.T.);
#9250=EDGE_CURVE('',#7183,#7184,#4823,.T.);
#9251=EDGE_CURVE('',#7184,#7181,#1295,.T.);
#9252=EDGE_CURVE('',#7185,#7186,#1296,.T.);
#9253=EDGE_CURVE('',#7186,#7187,#4824,.T.);
#9254=EDGE_CURVE('',#7187,#7188,#4825,.F.);
#9255=EDGE_CURVE('',#7188,#7189,#4826,.T.);
#9256=EDGE_CURVE('',#7189,#7185,#1297,.T.);
#9257=EDGE_CURVE('',#7189,#7190,#1911,.T.);
#9258=EDGE_CURVE('',#7191,#7190,#1298,.T.);
#9259=EDGE_CURVE('',#7191,#6555,#579,.T.);
#9260=EDGE_CURVE('',#7185,#6554,#580,.T.);
#9261=EDGE_CURVE('',#7188,#7192,#1912,.T.);
#9262=EDGE_CURVE('',#7190,#7192,#4827,.T.);
#9263=EDGE_CURVE('',#7193,#7192,#4828,.T.);
#9264=EDGE_CURVE('',#7193,#7194,#4829,.T.);
#9265=EDGE_CURVE('',#7194,#7191,#1299,.T.);
#9266=EDGE_CURVE('',#7195,#7196,#1300,.T.);
#9267=EDGE_CURVE('',#7196,#7197,#4830,.T.);
#9268=EDGE_CURVE('',#7197,#7198,#4831,.F.);
#9269=EDGE_CURVE('',#7198,#7199,#4832,.T.);
#9270=EDGE_CURVE('',#7199,#7195,#1301,.T.);
#9271=EDGE_CURVE('',#7199,#7200,#1913,.T.);
#9272=EDGE_CURVE('',#7201,#7200,#1302,.T.);
#9273=EDGE_CURVE('',#7201,#6557,#581,.T.);
#9274=EDGE_CURVE('',#7195,#6556,#582,.T.);
#9275=EDGE_CURVE('',#7198,#7202,#1914,.T.);
#9276=EDGE_CURVE('',#7200,#7202,#4833,.T.);
#9277=EDGE_CURVE('',#7203,#7202,#4834,.T.);
#9278=EDGE_CURVE('',#7203,#7204,#4835,.T.);
#9279=EDGE_CURVE('',#7204,#7201,#1303,.T.);
#9280=EDGE_CURVE('',#7205,#7206,#1304,.T.);
#9281=EDGE_CURVE('',#7206,#7207,#4836,.T.);
#9282=EDGE_CURVE('',#7207,#7208,#4837,.F.);
#9283=EDGE_CURVE('',#7208,#7209,#4838,.T.);
#9284=EDGE_CURVE('',#7209,#7205,#1305,.T.);
#9285=EDGE_CURVE('',#7209,#7210,#1915,.T.);
#9286=EDGE_CURVE('',#7211,#7210,#1306,.T.);
#9287=EDGE_CURVE('',#7211,#6559,#583,.T.);
#9288=EDGE_CURVE('',#7205,#6558,#584,.T.);
#9289=EDGE_CURVE('',#7208,#7212,#1916,.T.);
#9290=EDGE_CURVE('',#7210,#7212,#4839,.T.);
#9291=EDGE_CURVE('',#7213,#7212,#4840,.T.);
#9292=EDGE_CURVE('',#7213,#7214,#4841,.T.);
#9293=EDGE_CURVE('',#7214,#7211,#1307,.T.);
#9294=EDGE_CURVE('',#7215,#7216,#1308,.T.);
#9295=EDGE_CURVE('',#7216,#7217,#4842,.T.);
#9296=EDGE_CURVE('',#7217,#7218,#4843,.F.);
#9297=EDGE_CURVE('',#7218,#7219,#4844,.T.);
#9298=EDGE_CURVE('',#7219,#7215,#1309,.T.);
#9299=EDGE_CURVE('',#7219,#7220,#1917,.T.);
#9300=EDGE_CURVE('',#7221,#7220,#1310,.T.);
#9301=EDGE_CURVE('',#7221,#6561,#585,.T.);
#9302=EDGE_CURVE('',#7215,#6560,#586,.T.);
#9303=EDGE_CURVE('',#7218,#7222,#1918,.T.);
#9304=EDGE_CURVE('',#7220,#7222,#4845,.T.);
#9305=EDGE_CURVE('',#7223,#7224,#1311,.T.);
#9306=EDGE_CURVE('',#7224,#7225,#4846,.T.);
#9307=EDGE_CURVE('',#7225,#7226,#4847,.F.);
#9308=EDGE_CURVE('',#7226,#7223,#4848,.T.);
#9309=EDGE_CURVE('',#7227,#7224,#1919,.T.);
#9310=EDGE_CURVE('',#7228,#7227,#4849,.T.);
#9311=EDGE_CURVE('',#7225,#7228,#1920,.T.);
#9312=EDGE_CURVE('',#6562,#7223,#587,.T.);
#9313=EDGE_CURVE('',#7227,#7221,#1312,.T.);
#9314=EDGE_CURVE('',#7228,#7222,#4850,.T.);
#9315=EDGE_CURVE('',#7229,#7230,#4851,.T.);
#9316=EDGE_CURVE('',#7229,#7231,#4852,.T.);
#9317=EDGE_CURVE('',#7231,#7232,#1313,.T.);
#9318=EDGE_CURVE('',#7232,#7230,#4853,.T.);
#9319=EDGE_CURVE('',#7231,#7233,#1921,.T.);
#9320=EDGE_CURVE('',#7234,#7233,#1314,.T.);
#9321=EDGE_CURVE('',#6544,#7234,#588,.T.);
#9322=EDGE_CURVE('',#7232,#6543,#589,.T.);
#9323=EDGE_CURVE('',#7235,#7229,#1922,.T.);
#9324=EDGE_CURVE('',#7233,#7235,#4854,.T.);
#9325=EDGE_CURVE('',#7236,#7237,#4855,.T.);
#9326=EDGE_CURVE('',#7238,#7237,#4856,.T.);
#9327=EDGE_CURVE('',#7238,#7239,#4857,.T.);
#9328=EDGE_CURVE('',#7239,#7236,#590,.T.);
#9329=EDGE_CURVE('',#6545,#7236,#591,.T.);
#9330=EDGE_CURVE('',#7239,#7146,#1923,.T.);
#9331=EDGE_CURVE('',#7154,#7156,#1924,.T.);
#9332=EDGE_CURVE('',#7164,#7166,#1925,.T.);
#9333=EDGE_CURVE('',#7174,#7176,#1926,.T.);
#9334=EDGE_CURVE('',#7184,#7186,#1927,.T.);
#9335=EDGE_CURVE('',#7194,#7196,#1928,.T.);
#9336=EDGE_CURVE('',#7204,#7206,#1929,.T.);
#9337=EDGE_CURVE('',#7214,#7216,#1930,.T.);
#9338=EDGE_CURVE('',#7217,#7213,#1931,.T.);
#9339=EDGE_CURVE('',#7207,#7203,#1932,.T.);
#9340=EDGE_CURVE('',#7197,#7193,#1933,.T.);
#9341=EDGE_CURVE('',#7187,#7183,#1934,.T.);
#9342=EDGE_CURVE('',#7177,#7173,#1935,.T.);
#9343=EDGE_CURVE('',#7167,#7163,#1936,.T.);
#9344=EDGE_CURVE('',#7157,#7153,#1937,.T.);
#9345=EDGE_CURVE('',#7147,#7238,#1938,.T.);
#9346=EDGE_CURVE('',#7235,#7240,#4858,.F.);
#9347=EDGE_CURVE('',#7240,#7234,#4859,.T.);
#9348=EDGE_CURVE('',#7240,#7237,#1939,.T.);
#9349=EDGE_CURVE('',#7241,#7242,#4860,.T.);
#9350=EDGE_CURVE('',#7241,#7243,#4861,.T.);
#9351=EDGE_CURVE('',#7243,#6510,#1315,.T.);
#9352=EDGE_CURVE('',#6509,#7242,#4862,.T.);
#9353=EDGE_CURVE('',#7243,#7244,#1940,.T.);
#9354=EDGE_CURVE('',#7245,#7244,#1316,.T.);
#9355=EDGE_CURVE('',#7245,#6526,#592,.T.);
#9356=EDGE_CURVE('',#7246,#7241,#1941,.T.);
#9357=EDGE_CURVE('',#7244,#7246,#4863,.T.);
#9358=EDGE_CURVE('',#7246,#7247,#4864,.F.);
#9359=EDGE_CURVE('',#7247,#7248,#4865,.T.);
#9360=EDGE_CURVE('',#7248,#7245,#1317,.T.);
#9361=EDGE_CURVE('',#7249,#7250,#4866,.T.);
#9362=EDGE_CURVE('',#7249,#7251,#4867,.T.);
#9363=EDGE_CURVE('',#7251,#7252,#1318,.T.);
#9364=EDGE_CURVE('',#7252,#7253,#1319,.T.);
#9365=EDGE_CURVE('',#7253,#7250,#4868,.T.);
#9366=EDGE_CURVE('',#7251,#7254,#1942,.T.);
#9367=EDGE_CURVE('',#7255,#7254,#1320,.T.);
#9368=EDGE_CURVE('',#7255,#6528,#593,.T.);
#9369=EDGE_CURVE('',#7252,#6527,#594,.T.);
#9370=EDGE_CURVE('',#7256,#7249,#1943,.T.);
#9371=EDGE_CURVE('',#7254,#7256,#4869,.T.);
#9372=EDGE_CURVE('',#7256,#7257,#4870,.F.);
#9373=EDGE_CURVE('',#7257,#7258,#4871,.T.);
#9374=EDGE_CURVE('',#7258,#7255,#1321,.T.);
#9375=EDGE_CURVE('',#7259,#7260,#4872,.T.);
#9376=EDGE_CURVE('',#7259,#7261,#4873,.T.);
#9377=EDGE_CURVE('',#7261,#7262,#1322,.T.);
#9378=EDGE_CURVE('',#7262,#7263,#1323,.T.);
#9379=EDGE_CURVE('',#7263,#7260,#4874,.T.);
#9380=EDGE_CURVE('',#7261,#7264,#1944,.T.);
#9381=EDGE_CURVE('',#7265,#7264,#1324,.T.);
#9382=EDGE_CURVE('',#7265,#6530,#595,.T.);
#9383=EDGE_CURVE('',#7262,#6529,#596,.T.);
#9384=EDGE_CURVE('',#7266,#7259,#1945,.T.);
#9385=EDGE_CURVE('',#7264,#7266,#4875,.T.);
#9386=EDGE_CURVE('',#7266,#7267,#4876,.F.);
#9387=EDGE_CURVE('',#7267,#7268,#4877,.T.);
#9388=EDGE_CURVE('',#7268,#7265,#1325,.T.);
#9389=EDGE_CURVE('',#7269,#7270,#4878,.T.);
#9390=EDGE_CURVE('',#7269,#7271,#4879,.T.);
#9391=EDGE_CURVE('',#7271,#7272,#1326,.T.);
#9392=EDGE_CURVE('',#7272,#7273,#1327,.T.);
#9393=EDGE_CURVE('',#7273,#7270,#4880,.T.);
#9394=EDGE_CURVE('',#7271,#7274,#1946,.T.);
#9395=EDGE_CURVE('',#7275,#7274,#1328,.T.);
#9396=EDGE_CURVE('',#7275,#6532,#597,.T.);
#9397=EDGE_CURVE('',#7272,#6531,#598,.T.);
#9398=EDGE_CURVE('',#7276,#7269,#1947,.T.);
#9399=EDGE_CURVE('',#7274,#7276,#4881,.T.);
#9400=EDGE_CURVE('',#7276,#7277,#4882,.F.);
#9401=EDGE_CURVE('',#7277,#7278,#4883,.T.);
#9402=EDGE_CURVE('',#7278,#7275,#1329,.T.);
#9403=EDGE_CURVE('',#7279,#7280,#4884,.T.);
#9404=EDGE_CURVE('',#7279,#7281,#4885,.T.);
#9405=EDGE_CURVE('',#7281,#7282,#1330,.T.);
#9406=EDGE_CURVE('',#7282,#7283,#1331,.T.);
#9407=EDGE_CURVE('',#7283,#7280,#4886,.T.);
#9408=EDGE_CURVE('',#7281,#7284,#1948,.T.);
#9409=EDGE_CURVE('',#7285,#7284,#1332,.T.);
#9410=EDGE_CURVE('',#7285,#6534,#599,.T.);
#9411=EDGE_CURVE('',#7282,#6533,#600,.T.);
#9412=EDGE_CURVE('',#7286,#7279,#1949,.T.);
#9413=EDGE_CURVE('',#7284,#7286,#4887,.T.);
#9414=EDGE_CURVE('',#7286,#7287,#4888,.F.);
#9415=EDGE_CURVE('',#7287,#7288,#4889,.T.);
#9416=EDGE_CURVE('',#7288,#7285,#1333,.T.);
#9417=EDGE_CURVE('',#7289,#7290,#4890,.T.);
#9418=EDGE_CURVE('',#7289,#7291,#4891,.T.);
#9419=EDGE_CURVE('',#7291,#7292,#1334,.T.);
#9420=EDGE_CURVE('',#7292,#7293,#1335,.T.);
#9421=EDGE_CURVE('',#7293,#7290,#4892,.T.);
#9422=EDGE_CURVE('',#7291,#7294,#1950,.T.);
#9423=EDGE_CURVE('',#7295,#7294,#1336,.T.);
#9424=EDGE_CURVE('',#7295,#6536,#601,.T.);
#9425=EDGE_CURVE('',#7292,#6535,#602,.T.);
#9426=EDGE_CURVE('',#7296,#7289,#1951,.T.);
#9427=EDGE_CURVE('',#7294,#7296,#4893,.T.);
#9428=EDGE_CURVE('',#7296,#7297,#4894,.F.);
#9429=EDGE_CURVE('',#7297,#7298,#4895,.T.);
#9430=EDGE_CURVE('',#7298,#7295,#1337,.T.);
#9431=EDGE_CURVE('',#7299,#7300,#4896,.T.);
#9432=EDGE_CURVE('',#7299,#7301,#4897,.T.);
#9433=EDGE_CURVE('',#7301,#7302,#1338,.T.);
#9434=EDGE_CURVE('',#7302,#7303,#1339,.T.);
#9435=EDGE_CURVE('',#7303,#7300,#4898,.T.);
#9436=EDGE_CURVE('',#7301,#7304,#1952,.T.);
#9437=EDGE_CURVE('',#7305,#7304,#1340,.T.);
#9438=EDGE_CURVE('',#7305,#6538,#603,.T.);
#9439=EDGE_CURVE('',#7302,#6537,#604,.T.);
#9440=EDGE_CURVE('',#7306,#7299,#1953,.T.);
#9441=EDGE_CURVE('',#7304,#7306,#4899,.T.);
#9442=EDGE_CURVE('',#7306,#7307,#4900,.F.);
#9443=EDGE_CURVE('',#7307,#7308,#4901,.T.);
#9444=EDGE_CURVE('',#7308,#7305,#1341,.T.);
#9445=EDGE_CURVE('',#7309,#7310,#4902,.T.);
#9446=EDGE_CURVE('',#7309,#7311,#4903,.T.);
#9447=EDGE_CURVE('',#7311,#7312,#1342,.T.);
#9448=EDGE_CURVE('',#7312,#7313,#1343,.T.);
#9449=EDGE_CURVE('',#7313,#7310,#4904,.T.);
#9450=EDGE_CURVE('',#7311,#7314,#1954,.T.);
#9451=EDGE_CURVE('',#7315,#7314,#1344,.T.);
#9452=EDGE_CURVE('',#7315,#6540,#605,.T.);
#9453=EDGE_CURVE('',#7312,#6539,#606,.T.);
#9454=EDGE_CURVE('',#7316,#7309,#1955,.T.);
#9455=EDGE_CURVE('',#7314,#7316,#4905,.T.);
#9456=EDGE_CURVE('',#7316,#7317,#4906,.F.);
#9457=EDGE_CURVE('',#7317,#7318,#4907,.T.);
#9458=EDGE_CURVE('',#7318,#7315,#1345,.T.);
#9459=EDGE_CURVE('',#7319,#7320,#4908,.T.);
#9460=EDGE_CURVE('',#7319,#7321,#4909,.T.);
#9461=EDGE_CURVE('',#7321,#7322,#1346,.T.);
#9462=EDGE_CURVE('',#7322,#7323,#1347,.T.);
#9463=EDGE_CURVE('',#7323,#7320,#4910,.T.);
#9464=EDGE_CURVE('',#7321,#7324,#1956,.T.);
#9465=EDGE_CURVE('',#7325,#7324,#1348,.T.);
#9466=EDGE_CURVE('',#7325,#6542,#607,.T.);
#9467=EDGE_CURVE('',#7322,#6541,#608,.T.);
#9468=EDGE_CURVE('',#7326,#7319,#1957,.T.);
#9469=EDGE_CURVE('',#7324,#7326,#4911,.T.);
#9470=EDGE_CURVE('',#6344,#7327,#4912,.T.);
#9471=EDGE_CURVE('',#6347,#7328,#1349,.T.);
#9472=EDGE_CURVE('',#7328,#7327,#4913,.T.);
#9473=EDGE_CURVE('',#7329,#7328,#1958,.T.);
#9474=EDGE_CURVE('',#7330,#7329,#4914,.T.);
#9475=EDGE_CURVE('',#7330,#7327,#1959,.T.);
#9476=EDGE_CURVE('',#7329,#7325,#1350,.T.);
#9477=EDGE_CURVE('',#7326,#7330,#4915,.F.);
#9478=EDGE_CURVE('',#7248,#7253,#1960,.T.);
#9479=EDGE_CURVE('',#7258,#7263,#1961,.T.);
#9480=EDGE_CURVE('',#7268,#7273,#1962,.T.);
#9481=EDGE_CURVE('',#7278,#7283,#1963,.T.);
#9482=EDGE_CURVE('',#7288,#7293,#1964,.T.);
#9483=EDGE_CURVE('',#7298,#7303,#1965,.T.);
#9484=EDGE_CURVE('',#7308,#7313,#1966,.T.);
#9485=EDGE_CURVE('',#7318,#7323,#1967,.T.);
#9486=EDGE_CURVE('',#7317,#7320,#1968,.T.);
#9487=EDGE_CURVE('',#7307,#7310,#1969,.T.);
#9488=EDGE_CURVE('',#7297,#7300,#1970,.T.);
#9489=EDGE_CURVE('',#7287,#7290,#1971,.T.);
#9490=EDGE_CURVE('',#7277,#7280,#1972,.T.);
#9491=EDGE_CURVE('',#7267,#7270,#1973,.T.);
#9492=EDGE_CURVE('',#7257,#7260,#1974,.T.);
#9493=EDGE_CURVE('',#7247,#7250,#1975,.T.);
#9494=EDGE_CURVE('',#7331,#7331,#1976,.T.);
#9495=EDGE_CURVE('',#7331,#6662,#4916,.T.);
#9496=EDGE_CURVE('',#7332,#7332,#1977,.T.);
#9497=EDGE_CURVE('',#7332,#7331,#4917,.T.);
#9498=EDGE_CURVE('',#6412,#7333,#4918,.T.);
#9499=EDGE_CURVE('',#6409,#7333,#4919,.T.);
#9500=EDGE_CURVE('',#6407,#6417,#1978,.T.);
#9501=EDGE_CURVE('',#6424,#6429,#1979,.T.);
#9502=EDGE_CURVE('',#6436,#6441,#1980,.T.);
#9503=EDGE_CURVE('',#6448,#6453,#1981,.T.);
#9504=EDGE_CURVE('',#6460,#6465,#1982,.T.);
#9505=EDGE_CURVE('',#6472,#6477,#1983,.T.);
#9506=EDGE_CURVE('',#6484,#6489,#1984,.T.);
#9507=EDGE_CURVE('',#6496,#6501,#1985,.T.);
#9508=EDGE_CURVE('',#6507,#7242,#1986,.T.);
#9509=EDGE_CURVE('',#6495,#6498,#1987,.T.);
#9510=EDGE_CURVE('',#6483,#6486,#1988,.T.);
#9511=EDGE_CURVE('',#6471,#6474,#1989,.T.);
#9512=EDGE_CURVE('',#6459,#6462,#1990,.T.);
#9513=EDGE_CURVE('',#6447,#6450,#1991,.T.);
#9514=EDGE_CURVE('',#6435,#6438,#1992,.T.);
#9515=EDGE_CURVE('',#6423,#6426,#1993,.T.);
#9516=EDGE_CURVE('',#6406,#6414,#1994,.T.);
#9517=EDGE_CURVE('',#6400,#7334,#4920,.T.);
#9518=EDGE_CURVE('',#7334,#7335,#4921,.F.);
#9519=EDGE_CURVE('',#7335,#6401,#4922,.T.);
#9520=EDGE_CURVE('',#7335,#7333,#1995,.T.);
#9521=EDGE_CURVE('',#7336,#6664,#4923,.T.);
#9522=EDGE_CURVE('',#7336,#7337,#4924,.T.);
#9523=EDGE_CURVE('',#7337,#6665,#609,.T.);
#9524=EDGE_CURVE('',#7337,#7338,#1996,.T.);
#9525=EDGE_CURVE('',#7338,#7339,#610,.T.);
#9526=EDGE_CURVE('',#7339,#6516,#611,.T.);
#9527=EDGE_CURVE('',#7338,#7340,#4925,.T.);
#9528=EDGE_CURVE('',#7340,#7341,#4926,.F.);
#9529=EDGE_CURVE('',#7341,#7339,#4927,.T.);
#9530=EDGE_CURVE('',#7341,#7342,#1997,.T.);
#9531=EDGE_CURVE('',#7343,#7342,#4928,.T.);
#9532=EDGE_CURVE('',#6517,#7343,#612,.T.);
#9533=EDGE_CURVE('',#7344,#7345,#4929,.T.);
#9534=EDGE_CURVE('',#7346,#7345,#4930,.T.);
#9535=EDGE_CURVE('',#7346,#7347,#4931,.T.);
#9536=EDGE_CURVE('',#7347,#7344,#613,.T.);
#9537=EDGE_CURVE('',#7347,#7348,#1998,.T.);
#9538=EDGE_CURVE('',#7348,#6398,#614,.T.);
#9539=EDGE_CURVE('',#6525,#7344,#615,.T.);
#9540=EDGE_CURVE('',#7348,#7349,#4932,.T.);
#9541=EDGE_CURVE('',#7349,#6399,#4933,.F.);
#9542=EDGE_CURVE('',#7350,#6524,#616,.T.);
#9543=EDGE_CURVE('',#7351,#7350,#4934,.T.);
#9544=EDGE_CURVE('',#7351,#7345,#1999,.T.);
#9545=EDGE_CURVE('',#7352,#7342,#4935,.T.);
#9546=EDGE_CURVE('',#7352,#7353,#4936,.T.);
#9547=EDGE_CURVE('',#7353,#7343,#617,.T.);
#9548=EDGE_CURVE('',#7353,#7354,#2000,.T.);
#9549=EDGE_CURVE('',#7354,#7355,#618,.T.);
#9550=EDGE_CURVE('',#7355,#6518,#619,.T.);
#9551=EDGE_CURVE('',#7354,#7356,#4937,.T.);
#9552=EDGE_CURVE('',#7356,#7357,#4938,.F.);
#9553=EDGE_CURVE('',#7357,#7355,#4939,.T.);
#9554=EDGE_CURVE('',#7357,#7358,#2001,.T.);
#9555=EDGE_CURVE('',#7359,#7358,#4940,.T.);
#9556=EDGE_CURVE('',#6519,#7359,#620,.T.);
#9557=EDGE_CURVE('',#7360,#7361,#4941,.T.);
#9558=EDGE_CURVE('',#7362,#7361,#4942,.T.);
#9559=EDGE_CURVE('',#7362,#7363,#4943,.T.);
#9560=EDGE_CURVE('',#7363,#7360,#621,.T.);
#9561=EDGE_CURVE('',#7363,#7364,#2002,.T.);
#9562=EDGE_CURVE('',#7364,#7350,#622,.T.);
#9563=EDGE_CURVE('',#6523,#7360,#623,.T.);
#9564=EDGE_CURVE('',#7364,#7365,#4944,.T.);
#9565=EDGE_CURVE('',#7365,#7351,#4945,.F.);
#9566=EDGE_CURVE('',#7366,#6522,#624,.T.);
#9567=EDGE_CURVE('',#7367,#7366,#4946,.T.);
#9568=EDGE_CURVE('',#7367,#7361,#2003,.T.);
#9569=EDGE_CURVE('',#7368,#7358,#4947,.T.);
#9570=EDGE_CURVE('',#7368,#7369,#4948,.T.);
#9571=EDGE_CURVE('',#7369,#7359,#625,.T.);
#9572=EDGE_CURVE('',#7369,#7370,#2004,.T.);
#9573=EDGE_CURVE('',#7370,#7371,#626,.T.);
#9574=EDGE_CURVE('',#7371,#6520,#627,.T.);
#9575=EDGE_CURVE('',#7370,#7372,#4949,.T.);
#9576=EDGE_CURVE('',#7372,#7373,#4950,.F.);
#9577=EDGE_CURVE('',#7373,#7371,#4951,.T.);
#9578=EDGE_CURVE('',#7373,#7374,#2005,.T.);
#9579=EDGE_CURVE('',#7375,#7374,#4952,.T.);
#9580=EDGE_CURVE('',#6521,#7375,#628,.T.);
#9581=EDGE_CURVE('',#7376,#7374,#4953,.T.);
#9582=EDGE_CURVE('',#7376,#7377,#4954,.T.);
#9583=EDGE_CURVE('',#7377,#7375,#629,.T.);
#9584=EDGE_CURVE('',#7377,#7378,#2006,.T.);
#9585=EDGE_CURVE('',#7378,#7366,#630,.T.);
#9586=EDGE_CURVE('',#7378,#7379,#4955,.T.);
#9587=EDGE_CURVE('',#7379,#7367,#4956,.F.);
#9588=EDGE_CURVE('',#7380,#7380,#2007,.T.);
#9589=EDGE_CURVE('',#7380,#7381,#4957,.T.);
#9590=EDGE_CURVE('',#7381,#7381,#2008,.T.);
#9591=EDGE_CURVE('',#7382,#7382,#2009,.T.);
#9592=EDGE_CURVE('',#7380,#7383,#4958,.T.);
#9593=EDGE_CURVE('',#7383,#7379,#2010,.T.);
#9594=EDGE_CURVE('',#7379,#7376,#2011,.T.);
#9595=EDGE_CURVE('',#7376,#7372,#2012,.T.);
#9596=EDGE_CURVE('',#7372,#7368,#2013,.T.);
#9597=EDGE_CURVE('',#7368,#7356,#2014,.T.);
#9598=EDGE_CURVE('',#7356,#7352,#2015,.T.);
#9599=EDGE_CURVE('',#7352,#7340,#2016,.T.);
#9600=EDGE_CURVE('',#7340,#7336,#2017,.T.);
#9601=EDGE_CURVE('',#7336,#6666,#2018,.T.);
#9602=EDGE_CURVE('',#6666,#6390,#2019,.T.);
#9603=EDGE_CURVE('',#6390,#6380,#2020,.T.);
#9604=EDGE_CURVE('',#6380,#6388,#2021,.T.);
#9605=EDGE_CURVE('',#6388,#6364,#2022,.T.);
#9606=EDGE_CURVE('',#6364,#6372,#2023,.T.);
#9607=EDGE_CURVE('',#6372,#6350,#2024,.T.);
#9608=EDGE_CURVE('',#6354,#6696,#2025,.T.);
#9609=EDGE_CURVE('',#6698,#6689,#2026,.T.);
#9610=EDGE_CURVE('',#6685,#6679,#2027,.T.);
#9611=EDGE_CURVE('',#6675,#6669,#2028,.T.);
#9612=EDGE_CURVE('',#6758,#6755,#2029,.T.);
#9613=EDGE_CURVE('',#6748,#6745,#2030,.T.);
#9614=EDGE_CURVE('',#6738,#6735,#2031,.T.);
#9615=EDGE_CURVE('',#6728,#6725,#2032,.T.);
#9616=EDGE_CURVE('',#6718,#6715,#2033,.T.);
#9617=EDGE_CURVE('',#6708,#6705,#2034,.T.);
#9618=EDGE_CURVE('',#6699,#6801,#2035,.T.);
#9619=EDGE_CURVE('',#6804,#6793,#2036,.T.);
#9620=EDGE_CURVE('',#6789,#6783,#2037,.T.);
#9621=EDGE_CURVE('',#6779,#6773,#2038,.T.);
#9622=EDGE_CURVE('',#6769,#6763,#2039,.T.);
#9623=EDGE_CURVE('',#6854,#6851,#2040,.T.);
#9624=EDGE_CURVE('',#6844,#6841,#2041,.T.);
#9625=EDGE_CURVE('',#6834,#6831,#2042,.T.);
#9626=EDGE_CURVE('',#6824,#6821,#2043,.T.);
#9627=EDGE_CURVE('',#6814,#6811,#2044,.T.);
#9628=EDGE_CURVE('',#6805,#6907,#2045,.T.);
#9629=EDGE_CURVE('',#6910,#6899,#2046,.T.);
#9630=EDGE_CURVE('',#6895,#6889,#2047,.T.);
#9631=EDGE_CURVE('',#6885,#6879,#2048,.T.);
#9632=EDGE_CURVE('',#6875,#6869,#2049,.T.);
#9633=EDGE_CURVE('',#6865,#6859,#2050,.T.);
#9634=EDGE_CURVE('',#6950,#6947,#2051,.T.);
#9635=EDGE_CURVE('',#6940,#6937,#2052,.T.);
#9636=EDGE_CURVE('',#6930,#6927,#2053,.T.);
#9637=EDGE_CURVE('',#6920,#6917,#2054,.T.);
#9638=EDGE_CURVE('',#6911,#7013,#2055,.T.);
#9639=EDGE_CURVE('',#7016,#7005,#2056,.T.);
#9640=EDGE_CURVE('',#7001,#6995,#2057,.T.);
#9641=EDGE_CURVE('',#6991,#6985,#2058,.T.);
#9642=EDGE_CURVE('',#6981,#6975,#2059,.T.);
#9643=EDGE_CURVE('',#6971,#6965,#2060,.T.);
#9644=EDGE_CURVE('',#6961,#6955,#2061,.T.);
#9645=EDGE_CURVE('',#7046,#7043,#2062,.T.);
#9646=EDGE_CURVE('',#7036,#7033,#2063,.T.);
#9647=EDGE_CURVE('',#7026,#7023,#2064,.T.);
#9648=EDGE_CURVE('',#7017,#7119,#2065,.T.);
#9649=EDGE_CURVE('',#7122,#7111,#2066,.T.);
#9650=EDGE_CURVE('',#7107,#7101,#2067,.T.);
#9651=EDGE_CURVE('',#7097,#7091,#2068,.T.);
#9652=EDGE_CURVE('',#7087,#7081,#2069,.T.);
#9653=EDGE_CURVE('',#7077,#7071,#2070,.T.);
#9654=EDGE_CURVE('',#7067,#7061,#2071,.T.);
#9655=EDGE_CURVE('',#7057,#7051,#2072,.T.);
#9656=EDGE_CURVE('',#7142,#7139,#2073,.T.);
#9657=EDGE_CURVE('',#7132,#7129,#2074,.T.);
#9658=EDGE_CURVE('',#7123,#7225,#2075,.T.);
#9659=EDGE_CURVE('',#7228,#7217,#2076,.T.);
#9660=EDGE_CURVE('',#7213,#7207,#2077,.T.);
#9661=EDGE_CURVE('',#7203,#7197,#2078,.T.);
#9662=EDGE_CURVE('',#7193,#7187,#2079,.T.);
#9663=EDGE_CURVE('',#7183,#7177,#2080,.T.);
#9664=EDGE_CURVE('',#7173,#7167,#2081,.T.);
#9665=EDGE_CURVE('',#7163,#7157,#2082,.T.);
#9666=EDGE_CURVE('',#7153,#7147,#2083,.T.);
#9667=EDGE_CURVE('',#7238,#7235,#2084,.T.);
#9668=EDGE_CURVE('',#7229,#6341,#2085,.T.);
#9669=EDGE_CURVE('',#6344,#7326,#2086,.T.);
#9670=EDGE_CURVE('',#7319,#7316,#2087,.T.);
#9671=EDGE_CURVE('',#7309,#7306,#2088,.T.);
#9672=EDGE_CURVE('',#7299,#7296,#2089,.T.);
#9673=EDGE_CURVE('',#7289,#7286,#2090,.T.);
#9674=EDGE_CURVE('',#7279,#7276,#2091,.T.);
#9675=EDGE_CURVE('',#7269,#7266,#2092,.T.);
#9676=EDGE_CURVE('',#7259,#7256,#2093,.T.);
#9677=EDGE_CURVE('',#7249,#7246,#2094,.T.);
#9678=EDGE_CURVE('',#7241,#6506,#2095,.T.);
#9679=EDGE_CURVE('',#6497,#6494,#2096,.T.);
#9680=EDGE_CURVE('',#6485,#6482,#2097,.T.);
#9681=EDGE_CURVE('',#6473,#6470,#2098,.T.);
#9682=EDGE_CURVE('',#6461,#6458,#2099,.T.);
#9683=EDGE_CURVE('',#6449,#6446,#2100,.T.);
#9684=EDGE_CURVE('',#6437,#6434,#2101,.T.);
#9685=EDGE_CURVE('',#6425,#6422,#2102,.T.);
#9686=EDGE_CURVE('',#6413,#6405,#2103,.T.);
#9687=EDGE_CURVE('',#6409,#7334,#2104,.T.);
#9688=EDGE_CURVE('',#7334,#6392,#2105,.T.);
#9689=EDGE_CURVE('',#6392,#7349,#2106,.T.);
#9690=EDGE_CURVE('',#7349,#7346,#2107,.T.);
#9691=EDGE_CURVE('',#7346,#7365,#2108,.T.);
#9692=EDGE_CURVE('',#7365,#7362,#2109,.T.);
#9693=EDGE_CURVE('',#7362,#7383,#2110,.T.);
#9694=EDGE_CURVE('',#7384,#7384,#2111,.T.);
#9695=EDGE_CURVE('',#7384,#7385,#4959,.T.);
#9696=EDGE_CURVE('',#7385,#7385,#2112,.T.);
#9697=EDGE_CURVE('',#7386,#7386,#2113,.T.);
#9698=EDGE_CURVE('',#7387,#7387,#2114,.T.);
#9699=EDGE_CURVE('',#7388,#7388,#2115,.T.);
#9700=EDGE_CURVE('',#7389,#7389,#2116,.T.);
#9701=EDGE_CURVE('',#7390,#7390,#2117,.T.);
#9702=EDGE_CURVE('',#7391,#7391,#2118,.T.);
#9703=EDGE_CURVE('',#7385,#7392,#4960,.T.);
#9704=EDGE_CURVE('',#7392,#7392,#2119,.T.);
#9705=EDGE_CURVE('',#7387,#7393,#4961,.T.);
#9706=EDGE_CURVE('',#7393,#7393,#2120,.T.);
#9707=EDGE_CURVE('',#7393,#7394,#4962,.T.);
#9708=EDGE_CURVE('',#7394,#7394,#2121,.T.);
#9709=EDGE_CURVE('',#7391,#7395,#4963,.T.);
#9710=EDGE_CURVE('',#7395,#7395,#2122,.T.);
#9711=EDGE_CURVE('',#7395,#7396,#4964,.T.);
#9712=EDGE_CURVE('',#7396,#7396,#2123,.T.);
#9713=EDGE_CURVE('',#7388,#7397,#4965,.T.);
#9714=EDGE_CURVE('',#7397,#7397,#2124,.T.);
#9715=EDGE_CURVE('',#7397,#7398,#4966,.T.);
#9716=EDGE_CURVE('',#7398,#7398,#2125,.T.);
#9717=EDGE_CURVE('',#7390,#7399,#4967,.T.);
#9718=EDGE_CURVE('',#7399,#7399,#2126,.T.);
#9719=EDGE_CURVE('',#7399,#7400,#4968,.T.);
#9720=EDGE_CURVE('',#7400,#7400,#2127,.T.);
#9721=EDGE_CURVE('',#7382,#7401,#4969,.T.);
#9722=EDGE_CURVE('',#7401,#7401,#2128,.T.);
#9723=EDGE_CURVE('',#7401,#7386,#4970,.T.);
#9724=EDGE_CURVE('',#7014,#6912,#2129,.T.);
#9725=EDGE_CURVE('',#6908,#6806,#2130,.T.);
#9726=EDGE_CURVE('',#6802,#6700,#2131,.T.);
#9727=EDGE_CURVE('',#6342,#7230,#2132,.T.);
#9728=EDGE_CURVE('',#7226,#7124,#2133,.T.);
#9729=EDGE_CURVE('',#7120,#7018,#2134,.T.);
#9730=EDGE_CURVE('',#7402,#7402,#2135,.T.);
#9731=EDGE_CURVE('',#7402,#7403,#4971,.T.);
#9732=EDGE_CURVE('',#7404,#7404,#2136,.T.);
#9733=EDGE_CURVE('',#7404,#7405,#4972,.T.);
#9734=EDGE_CURVE('',#7406,#7406,#2137,.T.);
#9735=EDGE_CURVE('',#7406,#7407,#4973,.T.);
#9736=EDGE_CURVE('',#7408,#7408,#2138,.T.);
#9737=EDGE_CURVE('',#7408,#7409,#4974,.T.);
#9738=EDGE_CURVE('',#7410,#7410,#2139,.T.);
#9739=EDGE_CURVE('',#7410,#7411,#4975,.T.);
#9740=EDGE_CURVE('',#7389,#7412,#4976,.T.);
#9741=EDGE_CURVE('',#7412,#7412,#2140,.T.);
#9742=EDGE_CURVE('',#7413,#7414,#4977,.T.);
#9743=EDGE_CURVE('',#7414,#7415,#631,.T.);
#9744=EDGE_CURVE('',#7416,#7415,#2141,.F.);
#9745=EDGE_CURVE('',#7416,#7413,#632,.T.);
#9746=EDGE_CURVE('',#7417,#7418,#4978,.T.);
#9747=EDGE_CURVE('',#7418,#7414,#633,.T.);
#9748=EDGE_CURVE('',#7413,#7417,#634,.T.);
#9749=EDGE_CURVE('',#7419,#7420,#4979,.T.);
#9750=EDGE_CURVE('',#7420,#7418,#635,.T.);
#9751=EDGE_CURVE('',#7417,#7419,#636,.T.);
#9752=EDGE_CURVE('',#7421,#7422,#4980,.T.);
#9753=EDGE_CURVE('',#7422,#7420,#637,.T.);
#9754=EDGE_CURVE('',#7419,#7421,#638,.T.);
#9755=EDGE_CURVE('',#7423,#7424,#4981,.T.);
#9756=EDGE_CURVE('',#7424,#7422,#639,.T.);
#9757=EDGE_CURVE('',#7421,#7423,#640,.T.);
#9758=EDGE_CURVE('',#7425,#7426,#4982,.T.);
#9759=EDGE_CURVE('',#7426,#7424,#641,.T.);
#9760=EDGE_CURVE('',#7423,#7425,#642,.T.);
#9761=EDGE_CURVE('',#7427,#7428,#4983,.T.);
#9762=EDGE_CURVE('',#7428,#7426,#643,.T.);
#9763=EDGE_CURVE('',#7425,#7427,#644,.T.);
#9764=EDGE_CURVE('',#7429,#7430,#4984,.T.);
#9765=EDGE_CURVE('',#7430,#7428,#645,.T.);
#9766=EDGE_CURVE('',#7427,#7429,#646,.T.);
#9767=EDGE_CURVE('',#7431,#7432,#4985,.T.);
#9768=EDGE_CURVE('',#7432,#7430,#647,.T.);
#9769=EDGE_CURVE('',#7429,#7431,#648,.T.);
#9770=EDGE_CURVE('',#7433,#7434,#4986,.T.);
#9771=EDGE_CURVE('',#7434,#7432,#649,.T.);
#9772=EDGE_CURVE('',#7431,#7433,#650,.T.);
#9773=EDGE_CURVE('',#7435,#7436,#4987,.T.);
#9774=EDGE_CURVE('',#7436,#7434,#651,.T.);
#9775=EDGE_CURVE('',#7433,#7435,#652,.T.);
#9776=EDGE_CURVE('',#7437,#7438,#4988,.T.);
#9777=EDGE_CURVE('',#7437,#7439,#653,.T.);
#9778=EDGE_CURVE('',#7439,#7440,#2142,.T.);
#9779=EDGE_CURVE('',#7440,#7438,#654,.T.);
#9780=EDGE_CURVE('',#7441,#7442,#4989,.T.);
#9781=EDGE_CURVE('',#7442,#7443,#655,.T.);
#9782=EDGE_CURVE('',#7444,#7443,#2143,.T.);
#9783=EDGE_CURVE('',#7441,#7444,#656,.T.);
#9784=EDGE_CURVE('',#7445,#7446,#4990,.T.);
#9785=EDGE_CURVE('',#7446,#7442,#657,.T.);
#9786=EDGE_CURVE('',#7445,#7441,#658,.T.);
#9787=EDGE_CURVE('',#7447,#7448,#4991,.T.);
#9788=EDGE_CURVE('',#7448,#7446,#659,.T.);
#9789=EDGE_CURVE('',#7447,#7445,#660,.T.);
#9790=EDGE_CURVE('',#7449,#7450,#4992,.T.);
#9791=EDGE_CURVE('',#7450,#7448,#661,.T.);
#9792=EDGE_CURVE('',#7449,#7447,#662,.T.);
#9793=EDGE_CURVE('',#7451,#7452,#4993,.T.);
#9794=EDGE_CURVE('',#7452,#7450,#663,.T.);
#9795=EDGE_CURVE('',#7451,#7449,#664,.T.);
#9796=EDGE_CURVE('',#7453,#7454,#4994,.T.);
#9797=EDGE_CURVE('',#7454,#7452,#665,.T.);
#9798=EDGE_CURVE('',#7453,#7451,#666,.T.);
#9799=EDGE_CURVE('',#7455,#7456,#4995,.T.);
#9800=EDGE_CURVE('',#7456,#7454,#667,.T.);
#9801=EDGE_CURVE('',#7455,#7453,#668,.T.);
#9802=EDGE_CURVE('',#7457,#7458,#4996,.T.);
#9803=EDGE_CURVE('',#7458,#7456,#669,.T.);
#9804=EDGE_CURVE('',#7457,#7455,#670,.T.);
#9805=EDGE_CURVE('',#7459,#7460,#4997,.T.);
#9806=EDGE_CURVE('',#7460,#7458,#671,.T.);
#9807=EDGE_CURVE('',#7459,#7457,#672,.T.);
#9808=EDGE_CURVE('',#7461,#7462,#4998,.T.);
#9809=EDGE_CURVE('',#7462,#7460,#673,.T.);
#9810=EDGE_CURVE('',#7461,#7459,#674,.T.);
#9811=EDGE_CURVE('',#7463,#7464,#4999,.T.);
#9812=EDGE_CURVE('',#7464,#7462,#675,.T.);
#9813=EDGE_CURVE('',#7463,#7461,#676,.T.);
#9814=EDGE_CURVE('',#7465,#7466,#5000,.T.);
#9815=EDGE_CURVE('',#7467,#7465,#677,.T.);
#9816=EDGE_CURVE('',#7468,#7467,#2144,.T.);
#9817=EDGE_CURVE('',#7468,#7466,#678,.T.);
#9818=EDGE_CURVE('',#7466,#7464,#679,.T.);
#9819=EDGE_CURVE('',#7465,#7463,#680,.T.);
#9820=EDGE_CURVE('',#7443,#7440,#681,.T.);
#9821=EDGE_CURVE('',#7415,#7468,#682,.T.);
#9822=EDGE_CURVE('',#7438,#7436,#683,.T.);
#9823=EDGE_CURVE('',#7439,#7444,#684,.T.);
#9824=EDGE_CURVE('',#7435,#7437,#685,.T.);
#9825=EDGE_CURVE('',#7467,#7416,#686,.T.);
#9826=EDGE_CURVE('',#7469,#7469,#2145,.T.);
#9827=EDGE_CURVE('',#7470,#7470,#2146,.T.);
#9828=EDGE_CURVE('',#7470,#7469,#5001,.T.);
#9829=EDGE_CURVE('',#7471,#7471,#2147,.T.);
#9830=EDGE_CURVE('',#7472,#7472,#2148,.T.);
#9831=EDGE_CURVE('',#7472,#7471,#5002,.T.);
#9832=EDGE_CURVE('',#7473,#7473,#2149,.T.);
#9833=EDGE_CURVE('',#7473,#7472,#5003,.T.);
#9834=EDGE_CURVE('',#7474,#7475,#5004,.T.);
#9835=EDGE_CURVE('',#7474,#7476,#687,.T.);
#9836=EDGE_CURVE('',#7476,#7477,#2150,.F.);
#9837=EDGE_CURVE('',#7477,#7475,#688,.T.);
#9838=EDGE_CURVE('',#7478,#7479,#5005,.T.);
#9839=EDGE_CURVE('',#7478,#7474,#689,.T.);
#9840=EDGE_CURVE('',#7475,#7479,#690,.T.);
#9841=EDGE_CURVE('',#7480,#7481,#5006,.T.);
#9842=EDGE_CURVE('',#7480,#7478,#691,.T.);
#9843=EDGE_CURVE('',#7479,#7481,#692,.T.);
#9844=EDGE_CURVE('',#7482,#7483,#5007,.T.);
#9845=EDGE_CURVE('',#7482,#7480,#693,.T.);
#9846=EDGE_CURVE('',#7481,#7483,#694,.T.);
#9847=EDGE_CURVE('',#7484,#7485,#5008,.T.);
#9848=EDGE_CURVE('',#7484,#7482,#695,.T.);
#9849=EDGE_CURVE('',#7483,#7485,#696,.T.);
#9850=EDGE_CURVE('',#7486,#7487,#5009,.T.);
#9851=EDGE_CURVE('',#7486,#7484,#697,.T.);
#9852=EDGE_CURVE('',#7485,#7487,#698,.T.);
#9853=EDGE_CURVE('',#7488,#7489,#5010,.T.);
#9854=EDGE_CURVE('',#7488,#7490,#699,.T.);
#9855=EDGE_CURVE('',#7491,#7490,#2151,.T.);
#9856=EDGE_CURVE('',#7489,#7491,#700,.T.);
#9857=EDGE_CURVE('',#7492,#7493,#5011,.T.);
#9858=EDGE_CURVE('',#7492,#7488,#701,.T.);
#9859=EDGE_CURVE('',#7493,#7489,#702,.T.);
#9860=EDGE_CURVE('',#7494,#7495,#5012,.T.);
#9861=EDGE_CURVE('',#7494,#7492,#703,.T.);
#9862=EDGE_CURVE('',#7495,#7493,#704,.T.);
#9863=EDGE_CURVE('',#7496,#7497,#5013,.T.);
#9864=EDGE_CURVE('',#7496,#7494,#705,.T.);
#9865=EDGE_CURVE('',#7497,#7495,#706,.T.);
#9866=EDGE_CURVE('',#7498,#7499,#5014,.T.);
#9867=EDGE_CURVE('',#7498,#7496,#707,.T.);
#9868=EDGE_CURVE('',#7499,#7497,#708,.T.);
#9869=EDGE_CURVE('',#7500,#7501,#5015,.T.);
#9870=EDGE_CURVE('',#7500,#7498,#709,.T.);
#9871=EDGE_CURVE('',#7501,#7499,#710,.T.);
#9872=EDGE_CURVE('',#7490,#7502,#711,.T.);
#9873=EDGE_CURVE('',#7503,#7502,#2152,.F.);
#9874=EDGE_CURVE('',#7504,#7503,#2153,.F.);
#9875=EDGE_CURVE('',#7504,#7491,#712,.T.);
#9876=EDGE_CURVE('',#7487,#7504,#713,.T.);
#9877=EDGE_CURVE('',#7505,#7477,#714,.T.);
#9878=EDGE_CURVE('',#7505,#7501,#715,.T.);
#9879=EDGE_CURVE('',#7506,#7505,#2154,.T.);
#9880=EDGE_CURVE('',#7506,#7500,#716,.T.);
#9881=EDGE_CURVE('',#7476,#7506,#717,.T.);
#9882=EDGE_CURVE('',#7502,#7486,#718,.T.);
#9883=EDGE_CURVE('',#7502,#7504,#2155,.F.);
#9884=EDGE_CURVE('',#7507,#7507,#2156,.T.);
#9885=EDGE_CURVE('',#7508,#7508,#2157,.T.);
#9886=EDGE_CURVE('',#7508,#7507,#5016,.T.);
#9887=EDGE_CURVE('',#7509,#7509,#2158,.T.);
#9888=EDGE_CURVE('',#7509,#7508,#5017,.T.);
#9889=EDGE_CURVE('',#7510,#7510,#2159,.T.);
#9890=EDGE_CURVE('',#7510,#7503,#5018,.T.);
#9891=EDGE_CURVE('',#7511,#7512,#2160,.T.);
#9892=EDGE_CURVE('',#7512,#7511,#2161,.T.);
#9893=EDGE_CURVE('',#7511,#7513,#5019,.T.);
#9894=EDGE_CURVE('',#7513,#7514,#2162,.T.);
#9895=EDGE_CURVE('',#7514,#7513,#2163,.T.);
#9896=EDGE_CURVE('',#7514,#7515,#5020,.T.);
#9897=EDGE_CURVE('',#7515,#7515,#2164,.T.);
#9898=EDGE_CURVE('',#7516,#7516,#2165,.T.);
#9899=EDGE_CURVE('',#7516,#7512,#5021,.T.);
#9900=EDGE_CURVE('',#7517,#7517,#2166,.T.);
#9901=EDGE_CURVE('',#7518,#7518,#2167,.T.);
#9902=EDGE_CURVE('',#7517,#7519,#5022,.T.);
#9903=EDGE_CURVE('',#7519,#7519,#2168,.T.);
#9904=EDGE_CURVE('',#7518,#7520,#5023,.T.);
#9905=EDGE_CURVE('',#7520,#7520,#2169,.T.);
#9906=EDGE_CURVE('',#7521,#7521,#2170,.T.);
#9907=EDGE_CURVE('',#7521,#7522,#5024,.T.);
#9908=EDGE_CURVE('',#7522,#7522,#2171,.T.);
#9909=EDGE_CURVE('',#7523,#7523,#2172,.T.);
#9910=EDGE_CURVE('',#7515,#7523,#5025,.T.);
#9911=EDGE_CURVE('',#7524,#7524,#2173,.T.);
#9912=EDGE_CURVE('',#7524,#7525,#5026,.T.);
#9913=EDGE_CURVE('',#7525,#7525,#2174,.T.);
#9914=EDGE_CURVE('',#7526,#7526,#2175,.T.);
#9915=EDGE_CURVE('',#7527,#7527,#2176,.T.);
#9916=EDGE_CURVE('',#7527,#7526,#5027,.T.);
#9917=EDGE_CURVE('',#7528,#7528,#2177,.T.);
#9918=EDGE_CURVE('',#7528,#7529,#5028,.T.);
#9919=EDGE_CURVE('',#7529,#7530,#2178,.T.);
#9920=EDGE_CURVE('',#7530,#7529,#2179,.T.);
#9921=EDGE_CURVE('',#7530,#7531,#5029,.T.);
#9922=EDGE_CURVE('',#7531,#7531,#2180,.T.);
#9923=EDGE_CURVE('',#7532,#7532,#2181,.T.);
#9924=EDGE_CURVE('',#7532,#7533,#5030,.T.);
#9925=EDGE_CURVE('',#7533,#7533,#2182,.T.);
#9926=EDGE_CURVE('',#7534,#7534,#2183,.T.);
#9927=EDGE_CURVE('',#7531,#7534,#5031,.T.);
#9928=EDGE_CURVE('',#7535,#7535,#2184,.T.);
#9929=EDGE_CURVE('',#7535,#7536,#5032,.T.);
#9930=EDGE_CURVE('',#7536,#7536,#2185,.T.);
#9931=EDGE_CURVE('',#7536,#7537,#5033,.T.);
#9932=EDGE_CURVE('',#7537,#7537,#2186,.T.);
#9933=EDGE_CURVE('',#7538,#7538,#2187,.T.);
#9934=EDGE_CURVE('',#7539,#7539,#2188,.T.);
#9935=EDGE_CURVE('',#7539,#7537,#5034,.T.);
#9936=EDGE_CURVE('',#7540,#7540,#2189,.T.);
#9937=EDGE_CURVE('',#7540,#7541,#5035,.T.);
#9938=EDGE_CURVE('',#7541,#7542,#719,.T.);
#9939=EDGE_CURVE('',#7542,#7543,#2190,.T.);
#9940=EDGE_CURVE('',#7543,#7544,#720,.T.);
#9941=EDGE_CURVE('',#7544,#7545,#2191,.T.);
#9942=EDGE_CURVE('',#7545,#7546,#721,.T.);
#9943=EDGE_CURVE('',#7546,#7547,#2192,.T.);
#9944=EDGE_CURVE('',#7547,#7548,#722,.T.);
#9945=EDGE_CURVE('',#7548,#7549,#2193,.T.);
#9946=EDGE_CURVE('',#7549,#7550,#723,.T.);
#9947=EDGE_CURVE('',#7550,#7551,#2194,.T.);
#9948=EDGE_CURVE('',#7551,#7552,#724,.T.);
#9949=EDGE_CURVE('',#7552,#7553,#2195,.T.);
#9950=EDGE_CURVE('',#7553,#7541,#725,.T.);
#9951=EDGE_CURVE('',#7549,#7554,#726,.T.);
#9952=EDGE_CURVE('',#7554,#7555,#727,.F.);
#9953=EDGE_CURVE('',#7555,#7556,#728,.T.);
#9954=EDGE_CURVE('',#7556,#7557,#729,.F.);
#9955=EDGE_CURVE('',#7557,#7550,#730,.T.);
#9956=EDGE_CURVE('',#7547,#7558,#731,.T.);
#9957=EDGE_CURVE('',#7558,#7559,#732,.F.);
#9958=EDGE_CURVE('',#7559,#7560,#733,.T.);
#9959=EDGE_CURVE('',#7560,#7554,#734,.F.);
#9960=EDGE_CURVE('',#7554,#7548,#735,.T.);
#9961=EDGE_CURVE('',#7558,#7546,#736,.T.);
#9962=EDGE_CURVE('',#7561,#7544,#737,.T.);
#9963=EDGE_CURVE('',#7545,#7561,#738,.T.);
#9964=EDGE_CURVE('',#7562,#7542,#739,.T.);
#9965=EDGE_CURVE('',#7543,#7562,#740,.T.);
#9966=EDGE_CURVE('',#7563,#7552,#741,.T.);
#9967=EDGE_CURVE('',#7553,#7563,#742,.T.);
#9968=EDGE_CURVE('',#7551,#7557,#743,.T.);
#9969=EDGE_CURVE('',#7561,#7564,#744,.F.);
#9970=EDGE_CURVE('',#7564,#7565,#745,.T.);
#9971=EDGE_CURVE('',#7565,#7558,#746,.F.);
#9972=EDGE_CURVE('',#7559,#7565,#5036,.T.);
#9973=EDGE_CURVE('',#7566,#7561,#747,.F.);
#9974=EDGE_CURVE('',#7564,#7566,#5037,.T.);
#9975=EDGE_CURVE('',#7555,#7560,#5038,.T.);
#9976=EDGE_CURVE('',#7562,#7567,#748,.F.);
#9977=EDGE_CURVE('',#7568,#7562,#749,.F.);
#9978=EDGE_CURVE('',#7567,#7568,#5039,.T.);
#9979=EDGE_CURVE('',#7569,#7556,#5040,.T.);
#9980=EDGE_CURVE('',#7557,#7569,#750,.F.);
#9981=EDGE_CURVE('',#7563,#7570,#751,.F.);
#9982=EDGE_CURVE('',#7571,#7563,#752,.F.);
#9983=EDGE_CURVE('',#7570,#7571,#5041,.T.);
#9984=EDGE_CURVE('',#7569,#7571,#753,.T.);
#9985=EDGE_CURVE('',#7572,#7573,#1351,.T.);
#9986=EDGE_CURVE('',#7573,#7570,#5042,.T.);
#9987=EDGE_CURVE('',#7571,#7572,#5043,.T.);
#9988=EDGE_CURVE('',#7570,#7568,#754,.T.);
#9989=EDGE_CURVE('',#7574,#7575,#1352,.T.);
#9990=EDGE_CURVE('',#7575,#7569,#5044,.T.);
#9991=EDGE_CURVE('',#7556,#7574,#5045,.T.);
#9992=EDGE_CURVE('',#7576,#7577,#1353,.T.);
#9993=EDGE_CURVE('',#7577,#7567,#5046,.T.);
#9994=EDGE_CURVE('',#7568,#7576,#5047,.T.);
#9995=EDGE_CURVE('',#7567,#7566,#755,.T.);
#9996=EDGE_CURVE('',#7578,#7579,#1354,.T.);
#9997=EDGE_CURVE('',#7579,#7555,#5048,.T.);
#9998=EDGE_CURVE('',#7560,#7578,#5049,.T.);
#9999=EDGE_CURVE('',#7580,#7581,#1355,.T.);
#10000=EDGE_CURVE('',#7581,#7564,#5050,.T.);
#10001=EDGE_CURVE('',#7566,#7580,#5051,.T.);
#10002=EDGE_CURVE('',#7582,#7583,#1356,.T.);
#10003=EDGE_CURVE('',#7583,#7559,#5052,.T.);
#10004=EDGE_CURVE('',#7565,#7582,#5053,.T.);
#10005=EDGE_CURVE('',#7579,#7574,#1357,.T.);
#10006=EDGE_CURVE('',#7583,#7578,#1358,.T.);
#10007=EDGE_CURVE('',#7581,#7582,#1359,.T.);
#10008=EDGE_CURVE('',#7538,#7584,#5054,.T.);
#10009=EDGE_CURVE('',#7573,#7584,#1360,.T.);
#10010=EDGE_CURVE('',#7575,#7572,#1361,.T.);
#10011=EDGE_CURVE('',#7577,#7580,#1362,.T.);
#10012=EDGE_CURVE('',#7584,#7576,#1363,.T.);
#10013=EDGE_CURVE('',#7585,#7586,#2196,.T.);
#10014=EDGE_CURVE('',#7587,#7587,#2197,.T.);
#10015=EDGE_CURVE('',#7587,#7588,#756,.T.);
#10016=EDGE_CURVE('',#7588,#7588,#2198,.T.);
#10017=EDGE_CURVE('',#7589,#7590,#5055,.T.);
#10018=EDGE_CURVE('',#7589,#7591,#757,.T.);
#10019=EDGE_CURVE('',#7591,#7592,#2199,.T.);
#10020=EDGE_CURVE('',#7592,#7590,#758,.T.);
#10021=EDGE_CURVE('',#7593,#7594,#5056,.T.);
#10022=EDGE_CURVE('',#7593,#7589,#759,.T.);
#10023=EDGE_CURVE('',#7590,#7594,#760,.T.);
#10024=EDGE_CURVE('',#7595,#7596,#5057,.T.);
#10025=EDGE_CURVE('',#7595,#7593,#761,.T.);
#10026=EDGE_CURVE('',#7594,#7596,#762,.T.);
#10027=EDGE_CURVE('',#7597,#7598,#5058,.T.);
#10028=EDGE_CURVE('',#7597,#7595,#763,.T.);
#10029=EDGE_CURVE('',#7596,#7598,#764,.T.);
#10030=EDGE_CURVE('',#7599,#7600,#5059,.T.);
#10031=EDGE_CURVE('',#7599,#7601,#765,.T.);
#10032=EDGE_CURVE('',#7602,#7601,#2200,.T.);
#10033=EDGE_CURVE('',#7600,#7602,#766,.T.);
#10034=EDGE_CURVE('',#7603,#7604,#5060,.T.);
#10035=EDGE_CURVE('',#7603,#7599,#767,.T.);
#10036=EDGE_CURVE('',#7604,#7600,#768,.T.);
#10037=EDGE_CURVE('',#7605,#7606,#5061,.T.);
#10038=EDGE_CURVE('',#7605,#7603,#769,.T.);
#10039=EDGE_CURVE('',#7606,#7604,#770,.T.);
#10040=EDGE_CURVE('',#7607,#7608,#5062,.T.);
#10041=EDGE_CURVE('',#7607,#7605,#771,.T.);
#10042=EDGE_CURVE('',#7608,#7606,#772,.T.);
#10043=EDGE_CURVE('',#7601,#7609,#773,.T.);
#10044=EDGE_CURVE('',#7610,#7609,#2201,.F.);
#10045=EDGE_CURVE('',#7611,#7610,#2202,.F.);
#10046=EDGE_CURVE('',#7611,#7602,#774,.T.);
#10047=EDGE_CURVE('',#7598,#7611,#775,.T.);
#10048=EDGE_CURVE('',#7612,#7592,#776,.T.);
#10049=EDGE_CURVE('',#7612,#7608,#777,.T.);
#10050=EDGE_CURVE('',#7592,#7613,#2203,.T.);
#10051=EDGE_CURVE('',#7613,#7591,#2204,.T.);
#10052=EDGE_CURVE('',#7591,#7614,#778,.T.);
#10053=EDGE_CURVE('',#7614,#7612,#2205,.T.);
#10054=EDGE_CURVE('',#7614,#7607,#779,.T.);
#10055=EDGE_CURVE('',#7609,#7597,#780,.T.);
#10056=EDGE_CURVE('',#7615,#7616,#5063,.T.);
#10057=EDGE_CURVE('',#7615,#7617,#5064,.T.);
#10058=EDGE_CURVE('',#7617,#7618,#5065,.T.);
#10059=EDGE_CURVE('',#7616,#7618,#5066,.T.);
#10060=EDGE_CURVE('',#7619,#7615,#5067,.T.);
#10061=EDGE_CURVE('',#7619,#7620,#5068,.T.);
#10062=EDGE_CURVE('',#7620,#7617,#5069,.T.);
#10063=EDGE_CURVE('',#7621,#7619,#5070,.T.);
#10064=EDGE_CURVE('',#7621,#7622,#5071,.T.);
#10065=EDGE_CURVE('',#7622,#7620,#5072,.T.);
#10066=EDGE_CURVE('',#7623,#7621,#5073,.T.);
#10067=EDGE_CURVE('',#7623,#7624,#5074,.T.);
#10068=EDGE_CURVE('',#7624,#7622,#5075,.T.);
#10069=EDGE_CURVE('',#7625,#7623,#5076,.T.);
#10070=EDGE_CURVE('',#7625,#7626,#5077,.T.);
#10071=EDGE_CURVE('',#7626,#7624,#5078,.T.);
#10072=EDGE_CURVE('',#7616,#7625,#5079,.T.);
#10073=EDGE_CURVE('',#7618,#7626,#5080,.T.);
#10074=EDGE_CURVE('',#7627,#7627,#2206,.T.);
#10075=EDGE_CURVE('',#7613,#7627,#5081,.T.);
#10076=EDGE_CURVE('',#7609,#7611,#2207,.F.);
#10077=EDGE_CURVE('',#7628,#7628,#2208,.T.);
#10078=EDGE_CURVE('',#7628,#7610,#5082,.T.);
#10079=EDGE_CURVE('',#7629,#7630,#5083,.T.);
#10080=EDGE_CURVE('',#7629,#7631,#781,.T.);
#10081=EDGE_CURVE('',#7631,#7632,#2209,.T.);
#10082=EDGE_CURVE('',#7632,#7630,#782,.T.);
#10083=EDGE_CURVE('',#7633,#7634,#5084,.T.);
#10084=EDGE_CURVE('',#7633,#7629,#783,.T.);
#10085=EDGE_CURVE('',#7630,#7634,#784,.T.);
#10086=EDGE_CURVE('',#7635,#7636,#5085,.T.);
#10087=EDGE_CURVE('',#7635,#7633,#785,.T.);
#10088=EDGE_CURVE('',#7634,#7636,#786,.T.);
#10089=EDGE_CURVE('',#7637,#7638,#5086,.T.);
#10090=EDGE_CURVE('',#7637,#7635,#787,.T.);
#10091=EDGE_CURVE('',#7636,#7638,#788,.T.);
#10092=EDGE_CURVE('',#7639,#7640,#5087,.T.);
#10093=EDGE_CURVE('',#7639,#7637,#789,.T.);
#10094=EDGE_CURVE('',#7638,#7640,#790,.T.);
#10095=EDGE_CURVE('',#7641,#7642,#5088,.T.);
#10096=EDGE_CURVE('',#7641,#7639,#791,.T.);
#10097=EDGE_CURVE('',#7640,#7642,#792,.T.);
#10098=EDGE_CURVE('',#7643,#7644,#5089,.T.);
#10099=EDGE_CURVE('',#7643,#7641,#793,.T.);
#10100=EDGE_CURVE('',#7642,#7644,#794,.T.);
#10101=EDGE_CURVE('',#7645,#7646,#5090,.T.);
#10102=EDGE_CURVE('',#7645,#7643,#795,.T.);
#10103=EDGE_CURVE('',#7644,#7646,#796,.T.);
#10104=EDGE_CURVE('',#7647,#7648,#5091,.T.);
#10105=EDGE_CURVE('',#7647,#7645,#797,.T.);
#10106=EDGE_CURVE('',#7646,#7648,#798,.T.);
#10107=EDGE_CURVE('',#7649,#7650,#5092,.T.);
#10108=EDGE_CURVE('',#7649,#7647,#799,.T.);
#10109=EDGE_CURVE('',#7648,#7650,#800,.T.);
#10110=EDGE_CURVE('',#7651,#7652,#5093,.T.);
#10111=EDGE_CURVE('',#7651,#7649,#801,.T.);
#10112=EDGE_CURVE('',#7650,#7652,#802,.T.);
#10113=EDGE_CURVE('',#7653,#7654,#5094,.T.);
#10114=EDGE_CURVE('',#7653,#7651,#803,.T.);
#10115=EDGE_CURVE('',#7652,#7654,#804,.T.);
#10116=EDGE_CURVE('',#7655,#7656,#5095,.T.);
#10117=EDGE_CURVE('',#7655,#7653,#805,.T.);
#10118=EDGE_CURVE('',#7654,#7656,#806,.T.);
#10119=EDGE_CURVE('',#7657,#7658,#5096,.T.);
#10120=EDGE_CURVE('',#7657,#7655,#807,.T.);
#10121=EDGE_CURVE('',#7656,#7658,#808,.T.);
#10122=EDGE_CURVE('',#7659,#7660,#5097,.T.);
#10123=EDGE_CURVE('',#7659,#7657,#809,.T.);
#10124=EDGE_CURVE('',#7658,#7660,#810,.T.);
#10125=EDGE_CURVE('',#7661,#7662,#5098,.T.);
#10126=EDGE_CURVE('',#7661,#7663,#811,.T.);
#10127=EDGE_CURVE('',#7664,#7663,#2210,.T.);
#10128=EDGE_CURVE('',#7662,#7664,#812,.T.);
#10129=EDGE_CURVE('',#7665,#7666,#5099,.T.);
#10130=EDGE_CURVE('',#7665,#7661,#813,.T.);
#10131=EDGE_CURVE('',#7666,#7662,#814,.T.);
#10132=EDGE_CURVE('',#7667,#7668,#5100,.T.);
#10133=EDGE_CURVE('',#7667,#7665,#815,.T.);
#10134=EDGE_CURVE('',#7668,#7666,#816,.T.);
#10135=EDGE_CURVE('',#7669,#7670,#5101,.T.);
#10136=EDGE_CURVE('',#7669,#7667,#817,.T.);
#10137=EDGE_CURVE('',#7670,#7668,#818,.T.);
#10138=EDGE_CURVE('',#7671,#7672,#5102,.T.);
#10139=EDGE_CURVE('',#7671,#7669,#819,.T.);
#10140=EDGE_CURVE('',#7672,#7670,#820,.T.);
#10141=EDGE_CURVE('',#7673,#7674,#5103,.T.);
#10142=EDGE_CURVE('',#7673,#7671,#821,.T.);
#10143=EDGE_CURVE('',#7674,#7672,#822,.T.);
#10144=EDGE_CURVE('',#7675,#7676,#5104,.T.);
#10145=EDGE_CURVE('',#7675,#7673,#823,.T.);
#10146=EDGE_CURVE('',#7676,#7674,#824,.T.);
#10147=EDGE_CURVE('',#7677,#7678,#5105,.T.);
#10148=EDGE_CURVE('',#7677,#7675,#825,.T.);
#10149=EDGE_CURVE('',#7678,#7676,#826,.T.);
#10150=EDGE_CURVE('',#7679,#7680,#5106,.T.);
#10151=EDGE_CURVE('',#7679,#7677,#827,.T.);
#10152=EDGE_CURVE('',#7680,#7678,#828,.T.);
#10153=EDGE_CURVE('',#7681,#7682,#5107,.T.);
#10154=EDGE_CURVE('',#7681,#7679,#829,.T.);
#10155=EDGE_CURVE('',#7682,#7680,#830,.T.);
#10156=EDGE_CURVE('',#7683,#7684,#5108,.T.);
#10157=EDGE_CURVE('',#7683,#7681,#831,.T.);
#10158=EDGE_CURVE('',#7684,#7682,#832,.T.);
#10159=EDGE_CURVE('',#7685,#7686,#5109,.T.);
#10160=EDGE_CURVE('',#7685,#7683,#833,.T.);
#10161=EDGE_CURVE('',#7686,#7684,#834,.T.);
#10162=EDGE_CURVE('',#7687,#7688,#5110,.T.);
#10163=EDGE_CURVE('',#7687,#7685,#835,.T.);
#10164=EDGE_CURVE('',#7688,#7686,#836,.T.);
#10165=EDGE_CURVE('',#7689,#7690,#5111,.T.);
#10166=EDGE_CURVE('',#7689,#7687,#837,.T.);
#10167=EDGE_CURVE('',#7690,#7688,#838,.T.);
#10168=EDGE_CURVE('',#7691,#7664,#839,.T.);
#10169=EDGE_CURVE('',#7660,#7691,#840,.T.);
#10170=EDGE_CURVE('',#7692,#7632,#841,.T.);
#10171=EDGE_CURVE('',#7692,#7690,#842,.T.);
#10172=EDGE_CURVE('',#7632,#7693,#2211,.T.);
#10173=EDGE_CURVE('',#7693,#7631,#2212,.T.);
#10174=EDGE_CURVE('',#7631,#7694,#843,.T.);
#10175=EDGE_CURVE('',#7694,#7692,#2213,.T.);
#10176=EDGE_CURVE('',#7694,#7689,#844,.T.);
#10177=EDGE_CURVE('',#7663,#7695,#845,.T.);
#10178=EDGE_CURVE('',#7695,#7659,#846,.T.);
#10179=EDGE_CURVE('',#7696,#7697,#1364,.T.);
#10180=EDGE_CURVE('',#7698,#7696,#5112,.T.);
#10181=EDGE_CURVE('',#7699,#7698,#5113,.T.);
#10182=EDGE_CURVE('',#7697,#7699,#5114,.T.);
#10183=EDGE_CURVE('',#7699,#7700,#2214,.T.);
#10184=EDGE_CURVE('',#7698,#7700,#5115,.T.);
#10185=EDGE_CURVE('',#7701,#7696,#1365,.T.);
#10186=EDGE_CURVE('',#7700,#7701,#5116,.T.);
#10187=EDGE_CURVE('',#7702,#7701,#2215,.T.);
#10188=EDGE_CURVE('',#7702,#7703,#5117,.T.);
#10189=EDGE_CURVE('',#7703,#7704,#2216,.T.);
#10190=EDGE_CURVE('',#7704,#7705,#5118,.T.);
#10191=EDGE_CURVE('',#7706,#7705,#2217,.T.);
#10192=EDGE_CURVE('',#7706,#7707,#5119,.T.);
#10193=EDGE_CURVE('',#7707,#7708,#2218,.T.);
#10194=EDGE_CURVE('',#7708,#7709,#5120,.T.);
#10195=EDGE_CURVE('',#7710,#7709,#2219,.T.);
#10196=EDGE_CURVE('',#7710,#7711,#5121,.T.);
#10197=EDGE_CURVE('',#7711,#7712,#2220,.T.);
#10198=EDGE_CURVE('',#7712,#7713,#5122,.T.);
#10199=EDGE_CURVE('',#7714,#7713,#2221,.T.);
#10200=EDGE_CURVE('',#7714,#7715,#5123,.T.);
#10201=EDGE_CURVE('',#7715,#7716,#2222,.T.);
#10202=EDGE_CURVE('',#7716,#7717,#5124,.T.);
#10203=EDGE_CURVE('',#7718,#7717,#2223,.T.);
#10204=EDGE_CURVE('',#7718,#7719,#5125,.T.);
#10205=EDGE_CURVE('',#7719,#7720,#2224,.T.);
#10206=EDGE_CURVE('',#7720,#7721,#5126,.T.);
#10207=EDGE_CURVE('',#7722,#7721,#2225,.T.);
#10208=EDGE_CURVE('',#7722,#7723,#5127,.T.);
#10209=EDGE_CURVE('',#7723,#7724,#2226,.T.);
#10210=EDGE_CURVE('',#7724,#7725,#5128,.T.);
#10211=EDGE_CURVE('',#7726,#7725,#2227,.T.);
#10212=EDGE_CURVE('',#7726,#7727,#5129,.T.);
#10213=EDGE_CURVE('',#7727,#7728,#2228,.T.);
#10214=EDGE_CURVE('',#7728,#7729,#5130,.T.);
#10215=EDGE_CURVE('',#7730,#7729,#2229,.T.);
#10216=EDGE_CURVE('',#7730,#7731,#5131,.T.);
#10217=EDGE_CURVE('',#7731,#7732,#2230,.T.);
#10218=EDGE_CURVE('',#7732,#7733,#5132,.T.);
#10219=EDGE_CURVE('',#7734,#7733,#2231,.T.);
#10220=EDGE_CURVE('',#7734,#7735,#5133,.T.);
#10221=EDGE_CURVE('',#7735,#7736,#2232,.T.);
#10222=EDGE_CURVE('',#7736,#7737,#5134,.T.);
#10223=EDGE_CURVE('',#7738,#7737,#2233,.T.);
#10224=EDGE_CURVE('',#7738,#7739,#5135,.T.);
#10225=EDGE_CURVE('',#7739,#7740,#2234,.T.);
#10226=EDGE_CURVE('',#7740,#7741,#5136,.T.);
#10227=EDGE_CURVE('',#7742,#7741,#2235,.T.);
#10228=EDGE_CURVE('',#7742,#7743,#5137,.T.);
#10229=EDGE_CURVE('',#7743,#7744,#2236,.T.);
#10230=EDGE_CURVE('',#7744,#7745,#5138,.T.);
#10231=EDGE_CURVE('',#7746,#7745,#2237,.T.);
#10232=EDGE_CURVE('',#7746,#7747,#5139,.T.);
#10233=EDGE_CURVE('',#7747,#7748,#2238,.T.);
#10234=EDGE_CURVE('',#7748,#7749,#5140,.T.);
#10235=EDGE_CURVE('',#7750,#7749,#2239,.T.);
#10236=EDGE_CURVE('',#7750,#7751,#5141,.T.);
#10237=EDGE_CURVE('',#7751,#7752,#2240,.T.);
#10238=EDGE_CURVE('',#7752,#7753,#5142,.T.);
#10239=EDGE_CURVE('',#7754,#7753,#2241,.T.);
#10240=EDGE_CURVE('',#7754,#7755,#5143,.T.);
#10241=EDGE_CURVE('',#7755,#7756,#2242,.T.);
#10242=EDGE_CURVE('',#7756,#7757,#5144,.T.);
#10243=EDGE_CURVE('',#7757,#7757,#2243,.T.);
#10244=EDGE_CURVE('',#7756,#7758,#2244,.T.);
#10245=EDGE_CURVE('',#7758,#7759,#5145,.T.);
#10246=EDGE_CURVE('',#7760,#7759,#2245,.T.);
#10247=EDGE_CURVE('',#7760,#7761,#5146,.T.);
#10248=EDGE_CURVE('',#7761,#7762,#2246,.T.);
#10249=EDGE_CURVE('',#7762,#7763,#5147,.T.);
#10250=EDGE_CURVE('',#7764,#7763,#2247,.T.);
#10251=EDGE_CURVE('',#7764,#7765,#5148,.T.);
#10252=EDGE_CURVE('',#7765,#7766,#2248,.T.);
#10253=EDGE_CURVE('',#7766,#7767,#5149,.T.);
#10254=EDGE_CURVE('',#7768,#7767,#2249,.T.);
#10255=EDGE_CURVE('',#7768,#7769,#5150,.T.);
#10256=EDGE_CURVE('',#7769,#7770,#2250,.T.);
#10257=EDGE_CURVE('',#7770,#7771,#5151,.T.);
#10258=EDGE_CURVE('',#7772,#7771,#2251,.T.);
#10259=EDGE_CURVE('',#7772,#7773,#5152,.T.);
#10260=EDGE_CURVE('',#7773,#7774,#2252,.T.);
#10261=EDGE_CURVE('',#7774,#7775,#5153,.T.);
#10262=EDGE_CURVE('',#7776,#7775,#2253,.T.);
#10263=EDGE_CURVE('',#7776,#7777,#5154,.T.);
#10264=EDGE_CURVE('',#7777,#7778,#2254,.T.);
#10265=EDGE_CURVE('',#7778,#7779,#5155,.T.);
#10266=EDGE_CURVE('',#7780,#7779,#2255,.T.);
#10267=EDGE_CURVE('',#7780,#7781,#5156,.T.);
#10268=EDGE_CURVE('',#7781,#7782,#2256,.T.);
#10269=EDGE_CURVE('',#7782,#7783,#5157,.T.);
#10270=EDGE_CURVE('',#7784,#7783,#2257,.T.);
#10271=EDGE_CURVE('',#7784,#7785,#5158,.T.);
#10272=EDGE_CURVE('',#7785,#7786,#2258,.T.);
#10273=EDGE_CURVE('',#7786,#7787,#5159,.T.);
#10274=EDGE_CURVE('',#7788,#7787,#2259,.T.);
#10275=EDGE_CURVE('',#7788,#7789,#5160,.T.);
#10276=EDGE_CURVE('',#7789,#7790,#2260,.T.);
#10277=EDGE_CURVE('',#7790,#7791,#5161,.T.);
#10278=EDGE_CURVE('',#7792,#7791,#2261,.T.);
#10279=EDGE_CURVE('',#7792,#7793,#5162,.T.);
#10280=EDGE_CURVE('',#7793,#7794,#2262,.T.);
#10281=EDGE_CURVE('',#7794,#7795,#5163,.T.);
#10282=EDGE_CURVE('',#7796,#7795,#2263,.T.);
#10283=EDGE_CURVE('',#7796,#7797,#5164,.T.);
#10284=EDGE_CURVE('',#7797,#7798,#2264,.T.);
#10285=EDGE_CURVE('',#7798,#7799,#5165,.T.);
#10286=EDGE_CURVE('',#7800,#7799,#2265,.T.);
#10287=EDGE_CURVE('',#7800,#7801,#5166,.T.);
#10288=EDGE_CURVE('',#7801,#7802,#2266,.T.);
#10289=EDGE_CURVE('',#7802,#7803,#5167,.T.);
#10290=EDGE_CURVE('',#7804,#7803,#2267,.T.);
#10291=EDGE_CURVE('',#7804,#7805,#5168,.T.);
#10292=EDGE_CURVE('',#7805,#7806,#2268,.T.);
#10293=EDGE_CURVE('',#7806,#7807,#5169,.T.);
#10294=EDGE_CURVE('',#7808,#7807,#2269,.T.);
#10295=EDGE_CURVE('',#7808,#7809,#5170,.T.);
#10296=EDGE_CURVE('',#7809,#7810,#2270,.T.);
#10297=EDGE_CURVE('',#7810,#7811,#5171,.T.);
#10298=EDGE_CURVE('',#7812,#7811,#2271,.T.);
#10299=EDGE_CURVE('',#7812,#7813,#5172,.T.);
#10300=EDGE_CURVE('',#7813,#7814,#2272,.T.);
#10301=EDGE_CURVE('',#7814,#7815,#5173,.T.);
#10302=EDGE_CURVE('',#7816,#7815,#2273,.T.);
#10303=EDGE_CURVE('',#7816,#7817,#5174,.T.);
#10304=EDGE_CURVE('',#7817,#7818,#2274,.T.);
#10305=EDGE_CURVE('',#7818,#7819,#5175,.T.);
#10306=EDGE_CURVE('',#7697,#7819,#2275,.T.);
#10307=EDGE_CURVE('',#7820,#7702,#1366,.T.);
#10308=EDGE_CURVE('',#7821,#7820,#5176,.T.);
#10309=EDGE_CURVE('',#7703,#7821,#5177,.T.);
#10310=EDGE_CURVE('',#7821,#7704,#5178,.T.);
#10311=EDGE_CURVE('',#7705,#7820,#1367,.T.);
#10312=EDGE_CURVE('',#7822,#7706,#1368,.T.);
#10313=EDGE_CURVE('',#7823,#7822,#5179,.T.);
#10314=EDGE_CURVE('',#7707,#7823,#5180,.T.);
#10315=EDGE_CURVE('',#7823,#7708,#5181,.T.);
#10316=EDGE_CURVE('',#7709,#7822,#1369,.T.);
#10317=EDGE_CURVE('',#7824,#7710,#1370,.T.);
#10318=EDGE_CURVE('',#7825,#7824,#5182,.T.);
#10319=EDGE_CURVE('',#7711,#7825,#5183,.T.);
#10320=EDGE_CURVE('',#7825,#7712,#5184,.T.);
#10321=EDGE_CURVE('',#7713,#7824,#1371,.T.);
#10322=EDGE_CURVE('',#7826,#7714,#1372,.T.);
#10323=EDGE_CURVE('',#7827,#7826,#5185,.T.);
#10324=EDGE_CURVE('',#7715,#7827,#5186,.T.);
#10325=EDGE_CURVE('',#7827,#7716,#5187,.T.);
#10326=EDGE_CURVE('',#7717,#7826,#1373,.T.);
#10327=EDGE_CURVE('',#7828,#7718,#1374,.T.);
#10328=EDGE_CURVE('',#7829,#7828,#5188,.T.);
#10329=EDGE_CURVE('',#7719,#7829,#5189,.T.);
#10330=EDGE_CURVE('',#7829,#7720,#5190,.T.);
#10331=EDGE_CURVE('',#7721,#7828,#1375,.T.);
#10332=EDGE_CURVE('',#7830,#7722,#1376,.T.);
#10333=EDGE_CURVE('',#7831,#7830,#5191,.T.);
#10334=EDGE_CURVE('',#7723,#7831,#5192,.T.);
#10335=EDGE_CURVE('',#7831,#7724,#5193,.T.);
#10336=EDGE_CURVE('',#7725,#7830,#1377,.T.);
#10337=EDGE_CURVE('',#7832,#7726,#1378,.T.);
#10338=EDGE_CURVE('',#7833,#7832,#5194,.T.);
#10339=EDGE_CURVE('',#7727,#7833,#5195,.T.);
#10340=EDGE_CURVE('',#7833,#7728,#5196,.T.);
#10341=EDGE_CURVE('',#7729,#7832,#1379,.T.);
#10342=EDGE_CURVE('',#7834,#7730,#1380,.T.);
#10343=EDGE_CURVE('',#7835,#7834,#5197,.T.);
#10344=EDGE_CURVE('',#7731,#7835,#5198,.T.);
#10345=EDGE_CURVE('',#7835,#7732,#5199,.T.);
#10346=EDGE_CURVE('',#7733,#7834,#1381,.T.);
#10347=EDGE_CURVE('',#7836,#7734,#1382,.T.);
#10348=EDGE_CURVE('',#7837,#7836,#5200,.T.);
#10349=EDGE_CURVE('',#7735,#7837,#5201,.T.);
#10350=EDGE_CURVE('',#7837,#7736,#5202,.T.);
#10351=EDGE_CURVE('',#7737,#7836,#1383,.T.);
#10352=EDGE_CURVE('',#7838,#7738,#1384,.T.);
#10353=EDGE_CURVE('',#7839,#7838,#5203,.T.);
#10354=EDGE_CURVE('',#7739,#7839,#5204,.T.);
#10355=EDGE_CURVE('',#7839,#7740,#5205,.T.);
#10356=EDGE_CURVE('',#7741,#7838,#1385,.T.);
#10357=EDGE_CURVE('',#7840,#7742,#1386,.T.);
#10358=EDGE_CURVE('',#7841,#7840,#5206,.T.);
#10359=EDGE_CURVE('',#7743,#7841,#5207,.T.);
#10360=EDGE_CURVE('',#7841,#7744,#5208,.T.);
#10361=EDGE_CURVE('',#7745,#7840,#1387,.T.);
#10362=EDGE_CURVE('',#7842,#7746,#1388,.T.);
#10363=EDGE_CURVE('',#7843,#7842,#5209,.T.);
#10364=EDGE_CURVE('',#7747,#7843,#5210,.T.);
#10365=EDGE_CURVE('',#7843,#7748,#5211,.T.);
#10366=EDGE_CURVE('',#7749,#7842,#1389,.T.);
#10367=EDGE_CURVE('',#7844,#7750,#1390,.T.);
#10368=EDGE_CURVE('',#7845,#7844,#5212,.T.);
#10369=EDGE_CURVE('',#7751,#7845,#5213,.T.);
#10370=EDGE_CURVE('',#7845,#7752,#5214,.T.);
#10371=EDGE_CURVE('',#7753,#7844,#1391,.T.);
#10372=EDGE_CURVE('',#7846,#7754,#1392,.T.);
#10373=EDGE_CURVE('',#7847,#7846,#5215,.T.);
#10374=EDGE_CURVE('',#7755,#7847,#5216,.T.);
#10375=EDGE_CURVE('',#7847,#7758,#5217,.T.);
#10376=EDGE_CURVE('',#7759,#7846,#1393,.T.);
#10377=EDGE_CURVE('',#7848,#7760,#1394,.T.);
#10378=EDGE_CURVE('',#7849,#7848,#5218,.T.);
#10379=EDGE_CURVE('',#7761,#7849,#5219,.T.);
#10380=EDGE_CURVE('',#7849,#7762,#5220,.T.);
#10381=EDGE_CURVE('',#7763,#7848,#1395,.T.);
#10382=EDGE_CURVE('',#7850,#7764,#1396,.T.);
#10383=EDGE_CURVE('',#7851,#7850,#5221,.T.);
#10384=EDGE_CURVE('',#7765,#7851,#5222,.T.);
#10385=EDGE_CURVE('',#7851,#7766,#5223,.T.);
#10386=EDGE_CURVE('',#7767,#7850,#1397,.T.);
#10387=EDGE_CURVE('',#7852,#7768,#1398,.T.);
#10388=EDGE_CURVE('',#7853,#7852,#5224,.T.);
#10389=EDGE_CURVE('',#7769,#7853,#5225,.T.);
#10390=EDGE_CURVE('',#7853,#7770,#5226,.T.);
#10391=EDGE_CURVE('',#7771,#7852,#1399,.T.);
#10392=EDGE_CURVE('',#7854,#7772,#1400,.T.);
#10393=EDGE_CURVE('',#7855,#7854,#5227,.T.);
#10394=EDGE_CURVE('',#7773,#7855,#5228,.T.);
#10395=EDGE_CURVE('',#7855,#7774,#5229,.T.);
#10396=EDGE_CURVE('',#7775,#7854,#1401,.T.);
#10397=EDGE_CURVE('',#7856,#7776,#1402,.T.);
#10398=EDGE_CURVE('',#7857,#7856,#5230,.T.);
#10399=EDGE_CURVE('',#7777,#7857,#5231,.T.);
#10400=EDGE_CURVE('',#7857,#7778,#5232,.T.);
#10401=EDGE_CURVE('',#7779,#7856,#1403,.T.);
#10402=EDGE_CURVE('',#7858,#7780,#1404,.T.);
#10403=EDGE_CURVE('',#7859,#7858,#5233,.T.);
#10404=EDGE_CURVE('',#7781,#7859,#5234,.T.);
#10405=EDGE_CURVE('',#7859,#7782,#5235,.T.);
#10406=EDGE_CURVE('',#7783,#7858,#1405,.T.);
#10407=EDGE_CURVE('',#7860,#7784,#1406,.T.);
#10408=EDGE_CURVE('',#7861,#7860,#5236,.T.);
#10409=EDGE_CURVE('',#7785,#7861,#5237,.T.);
#10410=EDGE_CURVE('',#7861,#7786,#5238,.T.);
#10411=EDGE_CURVE('',#7787,#7860,#1407,.T.);
#10412=EDGE_CURVE('',#7862,#7788,#1408,.T.);
#10413=EDGE_CURVE('',#7863,#7862,#5239,.T.);
#10414=EDGE_CURVE('',#7789,#7863,#5240,.T.);
#10415=EDGE_CURVE('',#7863,#7790,#5241,.T.);
#10416=EDGE_CURVE('',#7791,#7862,#1409,.T.);
#10417=EDGE_CURVE('',#7864,#7792,#1410,.T.);
#10418=EDGE_CURVE('',#7865,#7864,#5242,.T.);
#10419=EDGE_CURVE('',#7793,#7865,#5243,.T.);
#10420=EDGE_CURVE('',#7865,#7794,#5244,.T.);
#10421=EDGE_CURVE('',#7795,#7864,#1411,.T.);
#10422=EDGE_CURVE('',#7866,#7796,#1412,.T.);
#10423=EDGE_CURVE('',#7867,#7866,#5245,.T.);
#10424=EDGE_CURVE('',#7797,#7867,#5246,.T.);
#10425=EDGE_CURVE('',#7867,#7798,#5247,.T.);
#10426=EDGE_CURVE('',#7799,#7866,#1413,.T.);
#10427=EDGE_CURVE('',#7868,#7800,#1414,.T.);
#10428=EDGE_CURVE('',#7869,#7868,#5248,.T.);
#10429=EDGE_CURVE('',#7801,#7869,#5249,.T.);
#10430=EDGE_CURVE('',#7869,#7802,#5250,.T.);
#10431=EDGE_CURVE('',#7803,#7868,#1415,.T.);
#10432=EDGE_CURVE('',#7870,#7804,#1416,.T.);
#10433=EDGE_CURVE('',#7871,#7870,#5251,.T.);
#10434=EDGE_CURVE('',#7805,#7871,#5252,.T.);
#10435=EDGE_CURVE('',#7871,#7806,#5253,.T.);
#10436=EDGE_CURVE('',#7807,#7870,#1417,.T.);
#10437=EDGE_CURVE('',#7872,#7808,#1418,.T.);
#10438=EDGE_CURVE('',#7873,#7872,#5254,.T.);
#10439=EDGE_CURVE('',#7809,#7873,#5255,.T.);
#10440=EDGE_CURVE('',#7873,#7810,#5256,.T.);
#10441=EDGE_CURVE('',#7811,#7872,#1419,.T.);
#10442=EDGE_CURVE('',#7874,#7812,#1420,.T.);
#10443=EDGE_CURVE('',#7875,#7874,#5257,.T.);
#10444=EDGE_CURVE('',#7813,#7875,#5258,.T.);
#10445=EDGE_CURVE('',#7875,#7814,#5259,.T.);
#10446=EDGE_CURVE('',#7815,#7874,#1421,.T.);
#10447=EDGE_CURVE('',#7876,#7816,#1422,.T.);
#10448=EDGE_CURVE('',#7877,#7876,#5260,.T.);
#10449=EDGE_CURVE('',#7817,#7877,#5261,.T.);
#10450=EDGE_CURVE('',#7877,#7818,#5262,.T.);
#10451=EDGE_CURVE('',#7819,#7876,#1423,.T.);
#10452=EDGE_CURVE('',#7878,#7878,#2276,.T.);
#10453=EDGE_CURVE('',#7693,#7878,#5263,.T.);
#10454=EDGE_CURVE('',#7695,#7691,#2277,.T.);
#10455=EDGE_CURVE('',#7879,#7879,#2278,.T.);
#10456=EDGE_CURVE('',#7757,#7879,#5264,.T.);
#10457=EDGE_CURVE('',#7880,#7880,#2279,.T.);
#10458=EDGE_CURVE('',#7880,#7846,#5265,.T.);
#10459=ORIENTED_EDGE('',*,*,#7881,.T.);
#10460=ORIENTED_EDGE('',*,*,#7882,.T.);
#10461=ORIENTED_EDGE('',*,*,#7883,.T.);
#10462=ORIENTED_EDGE('',*,*,#7884,.F.);
#10463=ORIENTED_EDGE('',*,*,#7885,.T.);
#10464=ORIENTED_EDGE('',*,*,#7886,.T.);
#10465=ORIENTED_EDGE('',*,*,#7887,.T.);
#10466=ORIENTED_EDGE('',*,*,#7888,.T.);
#10467=ORIENTED_EDGE('',*,*,#7889,.T.);
#10468=ORIENTED_EDGE('',*,*,#7886,.F.);
#10469=ORIENTED_EDGE('',*,*,#7890,.T.);
#10470=ORIENTED_EDGE('',*,*,#7884,.T.);
#10471=ORIENTED_EDGE('',*,*,#7891,.T.);
#10472=ORIENTED_EDGE('',*,*,#7888,.F.);
#10473=ORIENTED_EDGE('',*,*,#7892,.T.);
#10474=ORIENTED_EDGE('',*,*,#7882,.F.);
#10475=ORIENTED_EDGE('',*,*,#7892,.F.);
#10476=ORIENTED_EDGE('',*,*,#7893,.T.);
#10477=ORIENTED_EDGE('',*,*,#7894,.T.);
#10478=ORIENTED_EDGE('',*,*,#7895,.F.);
#10479=ORIENTED_EDGE('',*,*,#7887,.F.);
#10480=ORIENTED_EDGE('',*,*,#7896,.T.);
#10481=ORIENTED_EDGE('',*,*,#7897,.T.);
#10482=ORIENTED_EDGE('',*,*,#7893,.F.);
#10483=ORIENTED_EDGE('',*,*,#7898,.F.);
#10484=ORIENTED_EDGE('',*,*,#7899,.F.);
#10485=ORIENTED_EDGE('',*,*,#7900,.F.);
#10486=ORIENTED_EDGE('',*,*,#7901,.F.);
#10487=ORIENTED_EDGE('',*,*,#7902,.F.);
#10488=ORIENTED_EDGE('',*,*,#7903,.F.);
#10489=ORIENTED_EDGE('',*,*,#7904,.F.);
#10490=ORIENTED_EDGE('',*,*,#7905,.F.);
#10491=ORIENTED_EDGE('',*,*,#7906,.F.);
#10492=ORIENTED_EDGE('',*,*,#7907,.F.);
#10493=ORIENTED_EDGE('',*,*,#7908,.F.);
#10494=ORIENTED_EDGE('',*,*,#7909,.F.);
#10495=ORIENTED_EDGE('',*,*,#7910,.F.);
#10496=ORIENTED_EDGE('',*,*,#7911,.F.);
#10497=ORIENTED_EDGE('',*,*,#7912,.F.);
#10498=ORIENTED_EDGE('',*,*,#7913,.F.);
#10499=ORIENTED_EDGE('',*,*,#7914,.F.);
#10500=ORIENTED_EDGE('',*,*,#7885,.F.);
#10501=ORIENTED_EDGE('',*,*,#7891,.F.);
#10502=ORIENTED_EDGE('',*,*,#7881,.F.);
#10503=ORIENTED_EDGE('',*,*,#7890,.F.);
#10504=ORIENTED_EDGE('',*,*,#7915,.T.);
#10505=ORIENTED_EDGE('',*,*,#7916,.T.);
#10506=ORIENTED_EDGE('',*,*,#7914,.T.);
#10507=ORIENTED_EDGE('',*,*,#7917,.T.);
#10508=ORIENTED_EDGE('',*,*,#7918,.T.);
#10509=ORIENTED_EDGE('',*,*,#7917,.F.);
#10510=ORIENTED_EDGE('',*,*,#7913,.T.);
#10511=ORIENTED_EDGE('',*,*,#7919,.T.);
#10512=ORIENTED_EDGE('',*,*,#7912,.T.);
#10513=ORIENTED_EDGE('',*,*,#7920,.T.);
#10514=ORIENTED_EDGE('',*,*,#7921,.T.);
#10515=ORIENTED_EDGE('',*,*,#7919,.F.);
#10516=ORIENTED_EDGE('',*,*,#7915,.F.);
#10517=ORIENTED_EDGE('',*,*,#7922,.T.);
#10518=ORIENTED_EDGE('',*,*,#7923,.T.);
#10519=ORIENTED_EDGE('',*,*,#7924,.F.);
#10520=ORIENTED_EDGE('',*,*,#7918,.F.);
#10521=ORIENTED_EDGE('',*,*,#7925,.T.);
#10522=ORIENTED_EDGE('',*,*,#7926,.T.);
#10523=ORIENTED_EDGE('',*,*,#7922,.F.);
#10524=ORIENTED_EDGE('',*,*,#7921,.F.);
#10525=ORIENTED_EDGE('',*,*,#7927,.T.);
#10526=ORIENTED_EDGE('',*,*,#7928,.T.);
#10527=ORIENTED_EDGE('',*,*,#7925,.F.);
#10528=ORIENTED_EDGE('',*,*,#7929,.T.);
#10529=ORIENTED_EDGE('',*,*,#7930,.T.);
#10530=ORIENTED_EDGE('',*,*,#7931,.T.);
#10531=ORIENTED_EDGE('',*,*,#7910,.T.);
#10532=ORIENTED_EDGE('',*,*,#7930,.F.);
#10533=ORIENTED_EDGE('',*,*,#7932,.T.);
#10534=ORIENTED_EDGE('',*,*,#7933,.T.);
#10535=ORIENTED_EDGE('',*,*,#7934,.F.);
#10536=ORIENTED_EDGE('',*,*,#7935,.T.);
#10537=ORIENTED_EDGE('',*,*,#7936,.T.);
#10538=ORIENTED_EDGE('',*,*,#7937,.T.);
#10539=ORIENTED_EDGE('',*,*,#7908,.T.);
#10540=ORIENTED_EDGE('',*,*,#7936,.F.);
#10541=ORIENTED_EDGE('',*,*,#7938,.T.);
#10542=ORIENTED_EDGE('',*,*,#7939,.T.);
#10543=ORIENTED_EDGE('',*,*,#7940,.F.);
#10544=ORIENTED_EDGE('',*,*,#7941,.T.);
#10545=ORIENTED_EDGE('',*,*,#7942,.T.);
#10546=ORIENTED_EDGE('',*,*,#7943,.T.);
#10547=ORIENTED_EDGE('',*,*,#7906,.T.);
#10548=ORIENTED_EDGE('',*,*,#7942,.F.);
#10549=ORIENTED_EDGE('',*,*,#7944,.T.);
#10550=ORIENTED_EDGE('',*,*,#7945,.T.);
#10551=ORIENTED_EDGE('',*,*,#7946,.F.);
#10552=ORIENTED_EDGE('',*,*,#7947,.T.);
#10553=ORIENTED_EDGE('',*,*,#7948,.T.);
#10554=ORIENTED_EDGE('',*,*,#7949,.T.);
#10555=ORIENTED_EDGE('',*,*,#7904,.T.);
#10556=ORIENTED_EDGE('',*,*,#7948,.F.);
#10557=ORIENTED_EDGE('',*,*,#7950,.T.);
#10558=ORIENTED_EDGE('',*,*,#7951,.T.);
#10559=ORIENTED_EDGE('',*,*,#7952,.F.);
#10560=ORIENTED_EDGE('',*,*,#7953,.F.);
#10561=ORIENTED_EDGE('',*,*,#7954,.F.);
#10562=ORIENTED_EDGE('',*,*,#7955,.F.);
#10563=ORIENTED_EDGE('',*,*,#7956,.T.);
#10564=ORIENTED_EDGE('',*,*,#7900,.T.);
#10565=ORIENTED_EDGE('',*,*,#7954,.T.);
#10566=ORIENTED_EDGE('',*,*,#7957,.T.);
#10567=ORIENTED_EDGE('',*,*,#7958,.F.);
#10568=ORIENTED_EDGE('',*,*,#7959,.F.);
#10569=ORIENTED_EDGE('',*,*,#7960,.F.);
#10570=ORIENTED_EDGE('',*,*,#7961,.T.);
#10571=ORIENTED_EDGE('',*,*,#7962,.T.);
#10572=ORIENTED_EDGE('',*,*,#7959,.T.);
#10573=ORIENTED_EDGE('',*,*,#7898,.T.);
#10574=ORIENTED_EDGE('',*,*,#7963,.T.);
#10575=ORIENTED_EDGE('',*,*,#7964,.T.);
#10576=ORIENTED_EDGE('',*,*,#7960,.T.);
#10577=ORIENTED_EDGE('',*,*,#7965,.T.);
#10578=ORIENTED_EDGE('',*,*,#7966,.T.);
#10579=ORIENTED_EDGE('',*,*,#7958,.T.);
#10580=ORIENTED_EDGE('',*,*,#7967,.T.);
#10581=ORIENTED_EDGE('',*,*,#7955,.T.);
#10582=ORIENTED_EDGE('',*,*,#7899,.T.);
#10583=ORIENTED_EDGE('',*,*,#7968,.T.);
#10584=ORIENTED_EDGE('',*,*,#7969,.T.);
#10585=ORIENTED_EDGE('',*,*,#7953,.T.);
#10586=ORIENTED_EDGE('',*,*,#7970,.T.);
#10587=ORIENTED_EDGE('',*,*,#7971,.T.);
#10588=ORIENTED_EDGE('',*,*,#7957,.F.);
#10589=ORIENTED_EDGE('',*,*,#7969,.F.);
#10590=ORIENTED_EDGE('',*,*,#7972,.F.);
#10591=ORIENTED_EDGE('',*,*,#7973,.T.);
#10592=ORIENTED_EDGE('',*,*,#7974,.F.);
#10593=ORIENTED_EDGE('',*,*,#7968,.F.);
#10594=ORIENTED_EDGE('',*,*,#7975,.F.);
#10595=ORIENTED_EDGE('',*,*,#7976,.T.);
#10596=ORIENTED_EDGE('',*,*,#7977,.T.);
#10597=ORIENTED_EDGE('',*,*,#7972,.T.);
#10598=ORIENTED_EDGE('',*,*,#7978,.T.);
#10599=ORIENTED_EDGE('',*,*,#7979,.T.);
#10600=ORIENTED_EDGE('',*,*,#7973,.F.);
#10601=ORIENTED_EDGE('',*,*,#7977,.F.);
#10602=ORIENTED_EDGE('',*,*,#7980,.T.);
#10603=ORIENTED_EDGE('',*,*,#7978,.F.);
#10604=ORIENTED_EDGE('',*,*,#7981,.F.);
#10605=ORIENTED_EDGE('',*,*,#7982,.F.);
#10606=ORIENTED_EDGE('',*,*,#7983,.T.);
#10607=ORIENTED_EDGE('',*,*,#7984,.F.);
#10608=ORIENTED_EDGE('',*,*,#7985,.F.);
#10609=ORIENTED_EDGE('',*,*,#7986,.F.);
#10610=ORIENTED_EDGE('',*,*,#7987,.F.);
#10611=ORIENTED_EDGE('',*,*,#7980,.F.);
#10612=ORIENTED_EDGE('',*,*,#7976,.F.);
#10613=ORIENTED_EDGE('',*,*,#7988,.F.);
#10614=ORIENTED_EDGE('',*,*,#7989,.F.);
#10615=ORIENTED_EDGE('',*,*,#7990,.F.);
#10616=ORIENTED_EDGE('',*,*,#7985,.T.);
#10617=ORIENTED_EDGE('',*,*,#7991,.F.);
#10618=ORIENTED_EDGE('',*,*,#7981,.T.);
#10619=ORIENTED_EDGE('',*,*,#7992,.F.);
#10620=ORIENTED_EDGE('',*,*,#7993,.F.);
#10621=ORIENTED_EDGE('',*,*,#7994,.T.);
#10622=ORIENTED_EDGE('',*,*,#7995,.T.);
#10623=ORIENTED_EDGE('',*,*,#7986,.T.);
#10624=ORIENTED_EDGE('',*,*,#7990,.T.);
#10625=ORIENTED_EDGE('',*,*,#7996,.T.);
#10626=ORIENTED_EDGE('',*,*,#7997,.T.);
#10627=ORIENTED_EDGE('',*,*,#7920,.F.);
#10628=ORIENTED_EDGE('',*,*,#7911,.T.);
#10629=ORIENTED_EDGE('',*,*,#7916,.F.);
#10630=ORIENTED_EDGE('',*,*,#7997,.F.);
#10631=ORIENTED_EDGE('',*,*,#7924,.T.);
#10632=ORIENTED_EDGE('',*,*,#7998,.T.);
#10633=ORIENTED_EDGE('',*,*,#7927,.F.);
#10634=ORIENTED_EDGE('',*,*,#7999,.T.);
#10635=ORIENTED_EDGE('',*,*,#7935,.F.);
#10636=ORIENTED_EDGE('',*,*,#7907,.T.);
#10637=ORIENTED_EDGE('',*,*,#7931,.F.);
#10638=ORIENTED_EDGE('',*,*,#7999,.F.);
#10639=ORIENTED_EDGE('',*,*,#7934,.T.);
#10640=ORIENTED_EDGE('',*,*,#8000,.T.);
#10641=ORIENTED_EDGE('',*,*,#7938,.F.);
#10642=ORIENTED_EDGE('',*,*,#8001,.T.);
#10643=ORIENTED_EDGE('',*,*,#7929,.F.);
#10644=ORIENTED_EDGE('',*,*,#7909,.T.);
#10645=ORIENTED_EDGE('',*,*,#7937,.F.);
#10646=ORIENTED_EDGE('',*,*,#8001,.F.);
#10647=ORIENTED_EDGE('',*,*,#7940,.T.);
#10648=ORIENTED_EDGE('',*,*,#8002,.T.);
#10649=ORIENTED_EDGE('',*,*,#7932,.F.);
#10650=ORIENTED_EDGE('',*,*,#8003,.T.);
#10651=ORIENTED_EDGE('',*,*,#7947,.F.);
#10652=ORIENTED_EDGE('',*,*,#7903,.T.);
#10653=ORIENTED_EDGE('',*,*,#7943,.F.);
#10654=ORIENTED_EDGE('',*,*,#8003,.F.);
#10655=ORIENTED_EDGE('',*,*,#7946,.T.);
#10656=ORIENTED_EDGE('',*,*,#8004,.T.);
#10657=ORIENTED_EDGE('',*,*,#7950,.F.);
#10658=ORIENTED_EDGE('',*,*,#8005,.T.);
#10659=ORIENTED_EDGE('',*,*,#7941,.F.);
#10660=ORIENTED_EDGE('',*,*,#7905,.T.);
#10661=ORIENTED_EDGE('',*,*,#7949,.F.);
#10662=ORIENTED_EDGE('',*,*,#8005,.F.);
#10663=ORIENTED_EDGE('',*,*,#7952,.T.);
#10664=ORIENTED_EDGE('',*,*,#8006,.T.);
#10665=ORIENTED_EDGE('',*,*,#7944,.F.);
#10666=ORIENTED_EDGE('',*,*,#7992,.T.);
#10667=ORIENTED_EDGE('',*,*,#8007,.T.);
#10668=ORIENTED_EDGE('',*,*,#8008,.T.);
#10669=ORIENTED_EDGE('',*,*,#8007,.F.);
#10670=ORIENTED_EDGE('',*,*,#8008,.F.);
#10671=ORIENTED_EDGE('',*,*,#8009,.T.);
#10672=ORIENTED_EDGE('',*,*,#8010,.T.);
#10673=ORIENTED_EDGE('',*,*,#8009,.F.);
#10674=ORIENTED_EDGE('',*,*,#7966,.F.);
#10675=ORIENTED_EDGE('',*,*,#8011,.T.);
#10676=ORIENTED_EDGE('',*,*,#7996,.F.);
#10677=ORIENTED_EDGE('',*,*,#7989,.T.);
#10678=ORIENTED_EDGE('',*,*,#8012,.T.);
#10679=ORIENTED_EDGE('',*,*,#7962,.F.);
#10680=ORIENTED_EDGE('',*,*,#8013,.F.);
#10681=ORIENTED_EDGE('',*,*,#7994,.F.);
#10682=ORIENTED_EDGE('',*,*,#8011,.F.);
#10683=ORIENTED_EDGE('',*,*,#7965,.F.);
#10684=ORIENTED_EDGE('',*,*,#7963,.F.);
#10685=ORIENTED_EDGE('',*,*,#8012,.F.);
#10686=ORIENTED_EDGE('',*,*,#7988,.T.);
#10687=ORIENTED_EDGE('',*,*,#7975,.T.);
#10688=ORIENTED_EDGE('',*,*,#7971,.F.);
#10689=ORIENTED_EDGE('',*,*,#8014,.T.);
#10690=ORIENTED_EDGE('',*,*,#7964,.F.);
#10691=ORIENTED_EDGE('',*,*,#8014,.F.);
#10692=ORIENTED_EDGE('',*,*,#7970,.F.);
#10693=ORIENTED_EDGE('',*,*,#7967,.F.);
#10694=ORIENTED_EDGE('',*,*,#7984,.T.);
#10695=ORIENTED_EDGE('',*,*,#8015,.T.);
#10696=ORIENTED_EDGE('',*,*,#7982,.T.);
#10697=ORIENTED_EDGE('',*,*,#7991,.T.);
#10698=ORIENTED_EDGE('',*,*,#8015,.F.);
#10699=ORIENTED_EDGE('',*,*,#7983,.F.);
#10700=ORIENTED_EDGE('',*,*,#8016,.T.);
#10701=ORIENTED_EDGE('',*,*,#8017,.T.);
#10702=ORIENTED_EDGE('',*,*,#8018,.T.);
#10703=ORIENTED_EDGE('',*,*,#8019,.T.);
#10704=ORIENTED_EDGE('',*,*,#8018,.F.);
#10705=ORIENTED_EDGE('',*,*,#8020,.F.);
#10706=ORIENTED_EDGE('',*,*,#8021,.T.);
#10707=ORIENTED_EDGE('',*,*,#8017,.F.);
#10708=ORIENTED_EDGE('',*,*,#8021,.F.);
#10709=ORIENTED_EDGE('',*,*,#8019,.F.);
#10710=ORIENTED_EDGE('',*,*,#8022,.T.);
#10711=ORIENTED_EDGE('',*,*,#7901,.T.);
#10712=ORIENTED_EDGE('',*,*,#7956,.F.);
#10713=ORIENTED_EDGE('',*,*,#7974,.T.);
#10714=ORIENTED_EDGE('',*,*,#7979,.F.);
#10715=ORIENTED_EDGE('',*,*,#7987,.T.);
#10716=ORIENTED_EDGE('',*,*,#7995,.F.);
#10717=ORIENTED_EDGE('',*,*,#8013,.T.);
#10718=ORIENTED_EDGE('',*,*,#7961,.F.);
#10719=ORIENTED_EDGE('',*,*,#7902,.T.);
#10720=ORIENTED_EDGE('',*,*,#8022,.F.);
#10721=ORIENTED_EDGE('',*,*,#7993,.T.);
#10722=ORIENTED_EDGE('',*,*,#8023,.T.);
#10723=ORIENTED_EDGE('',*,*,#8024,.T.);
#10724=ORIENTED_EDGE('',*,*,#8023,.F.);
#10725=ORIENTED_EDGE('',*,*,#8025,.F.);
#10726=ORIENTED_EDGE('',*,*,#8026,.T.);
#10727=ORIENTED_EDGE('',*,*,#8024,.F.);
#10728=ORIENTED_EDGE('',*,*,#8026,.F.);
#10729=ORIENTED_EDGE('',*,*,#8020,.T.);
#10730=ORIENTED_EDGE('',*,*,#8027,.T.);
#10731=ORIENTED_EDGE('',*,*,#8028,.T.);
#10732=ORIENTED_EDGE('',*,*,#8027,.F.);
#10733=ORIENTED_EDGE('',*,*,#8028,.F.);
#10734=ORIENTED_EDGE('',*,*,#8029,.F.);
#10735=ORIENTED_EDGE('',*,*,#8030,.T.);
#10736=ORIENTED_EDGE('',*,*,#8031,.T.);
#10737=ORIENTED_EDGE('',*,*,#8029,.T.);
#10738=ORIENTED_EDGE('',*,*,#8032,.T.);
#10739=ORIENTED_EDGE('',*,*,#8025,.T.);
#10740=ORIENTED_EDGE('',*,*,#8032,.F.);
#10741=ORIENTED_EDGE('',*,*,#8016,.F.);
#10742=ORIENTED_EDGE('',*,*,#8033,.T.);
#10743=ORIENTED_EDGE('',*,*,#8034,.T.);
#10744=ORIENTED_EDGE('',*,*,#8033,.F.);
#10745=ORIENTED_EDGE('',*,*,#8034,.F.);
#10746=ORIENTED_EDGE('',*,*,#8010,.F.);
#10747=ORIENTED_EDGE('',*,*,#8035,.F.);
#10748=ORIENTED_EDGE('',*,*,#8031,.F.);
#10749=ORIENTED_EDGE('',*,*,#8036,.T.);
#10750=ORIENTED_EDGE('',*,*,#8035,.T.);
#10751=ORIENTED_EDGE('',*,*,#8036,.F.);
#10752=ORIENTED_EDGE('',*,*,#8030,.F.);
#10753=ORIENTED_EDGE('',*,*,#8037,.T.);
#10754=ORIENTED_EDGE('',*,*,#8038,.T.);
#10755=ORIENTED_EDGE('',*,*,#8037,.F.);
#10756=ORIENTED_EDGE('',*,*,#8038,.F.);
#10757=ORIENTED_EDGE('',*,*,#7945,.F.);
#10758=ORIENTED_EDGE('',*,*,#8006,.F.);
#10759=ORIENTED_EDGE('',*,*,#7951,.F.);
#10760=ORIENTED_EDGE('',*,*,#8004,.F.);
#10761=ORIENTED_EDGE('',*,*,#7933,.F.);
#10762=ORIENTED_EDGE('',*,*,#8002,.F.);
#10763=ORIENTED_EDGE('',*,*,#7939,.F.);
#10764=ORIENTED_EDGE('',*,*,#8000,.F.);
#10765=ORIENTED_EDGE('',*,*,#7928,.F.);
#10766=ORIENTED_EDGE('',*,*,#7998,.F.);
#10767=ORIENTED_EDGE('',*,*,#7923,.F.);
#10768=ORIENTED_EDGE('',*,*,#7926,.F.);
#10769=ORIENTED_EDGE('',*,*,#7889,.F.);
#10770=ORIENTED_EDGE('',*,*,#8039,.T.);
#10771=ORIENTED_EDGE('',*,*,#8040,.T.);
#10772=ORIENTED_EDGE('',*,*,#7896,.F.);
#10773=ORIENTED_EDGE('',*,*,#7883,.F.);
#10774=ORIENTED_EDGE('',*,*,#7895,.T.);
#10775=ORIENTED_EDGE('',*,*,#8041,.T.);
#10776=ORIENTED_EDGE('',*,*,#8039,.F.);
#10777=ORIENTED_EDGE('',*,*,#7894,.F.);
#10778=ORIENTED_EDGE('',*,*,#7897,.F.);
#10779=ORIENTED_EDGE('',*,*,#8040,.F.);
#10780=ORIENTED_EDGE('',*,*,#8041,.F.);
#10781=ORIENTED_EDGE('',*,*,#8042,.T.);
#10782=ORIENTED_EDGE('',*,*,#8043,.T.);
#10783=ORIENTED_EDGE('',*,*,#8044,.T.);
#10784=ORIENTED_EDGE('',*,*,#8045,.T.);
#10785=ORIENTED_EDGE('',*,*,#8043,.F.);
#10786=ORIENTED_EDGE('',*,*,#8046,.F.);
#10787=ORIENTED_EDGE('',*,*,#8047,.F.);
#10788=ORIENTED_EDGE('',*,*,#8048,.F.);
#10789=ORIENTED_EDGE('',*,*,#8042,.F.);
#10790=ORIENTED_EDGE('',*,*,#8049,.F.);
#10791=ORIENTED_EDGE('',*,*,#8050,.T.);
#10792=ORIENTED_EDGE('',*,*,#8051,.T.);
#10793=ORIENTED_EDGE('',*,*,#8052,.F.);
#10794=ORIENTED_EDGE('',*,*,#8046,.T.);
#10795=ORIENTED_EDGE('',*,*,#8053,.T.);
#10796=ORIENTED_EDGE('',*,*,#8054,.T.);
#10797=ORIENTED_EDGE('',*,*,#8055,.T.);
#10798=ORIENTED_EDGE('',*,*,#8056,.T.);
#10799=ORIENTED_EDGE('',*,*,#8057,.T.);
#10800=ORIENTED_EDGE('',*,*,#8054,.F.);
#10801=ORIENTED_EDGE('',*,*,#8058,.F.);
#10802=ORIENTED_EDGE('',*,*,#8059,.F.);
#10803=ORIENTED_EDGE('',*,*,#8060,.F.);
#10804=ORIENTED_EDGE('',*,*,#8053,.F.);
#10805=ORIENTED_EDGE('',*,*,#8061,.T.);
#10806=ORIENTED_EDGE('',*,*,#8062,.T.);
#10807=ORIENTED_EDGE('',*,*,#8063,.F.);
#10808=ORIENTED_EDGE('',*,*,#8064,.F.);
#10809=ORIENTED_EDGE('',*,*,#8058,.T.);
#10810=ORIENTED_EDGE('',*,*,#8065,.F.);
#10811=ORIENTED_EDGE('',*,*,#8059,.T.);
#10812=ORIENTED_EDGE('',*,*,#8064,.T.);
#10813=ORIENTED_EDGE('',*,*,#8066,.T.);
#10814=ORIENTED_EDGE('',*,*,#8066,.F.);
#10815=ORIENTED_EDGE('',*,*,#8063,.T.);
#10816=ORIENTED_EDGE('',*,*,#8067,.F.);
#10817=ORIENTED_EDGE('',*,*,#8068,.T.);
#10818=ORIENTED_EDGE('',*,*,#8069,.F.);
#10819=ORIENTED_EDGE('',*,*,#8070,.T.);
#10820=ORIENTED_EDGE('',*,*,#8071,.T.);
#10821=ORIENTED_EDGE('',*,*,#8072,.T.);
#10822=ORIENTED_EDGE('',*,*,#8073,.T.);
#10823=ORIENTED_EDGE('',*,*,#8074,.T.);
#10824=ORIENTED_EDGE('',*,*,#8075,.T.);
#10825=ORIENTED_EDGE('',*,*,#8075,.F.);
#10826=ORIENTED_EDGE('',*,*,#8076,.T.);
#10827=ORIENTED_EDGE('',*,*,#8077,.F.);
#10828=ORIENTED_EDGE('',*,*,#8078,.T.);
#10829=ORIENTED_EDGE('',*,*,#8079,.T.);
#10830=ORIENTED_EDGE('',*,*,#8080,.F.);
#10831=ORIENTED_EDGE('',*,*,#8074,.F.);
#10832=ORIENTED_EDGE('',*,*,#8081,.T.);
#10833=ORIENTED_EDGE('',*,*,#8082,.F.);
#10834=ORIENTED_EDGE('',*,*,#8076,.F.);
#10835=ORIENTED_EDGE('',*,*,#8083,.F.);
#10836=ORIENTED_EDGE('',*,*,#8084,.T.);
#10837=ORIENTED_EDGE('',*,*,#8085,.T.);
#10838=ORIENTED_EDGE('',*,*,#8086,.T.);
#10839=ORIENTED_EDGE('',*,*,#8087,.T.);
#10840=ORIENTED_EDGE('',*,*,#8056,.F.);
#10841=ORIENTED_EDGE('',*,*,#8088,.T.);
#10842=ORIENTED_EDGE('',*,*,#8087,.F.);
#10843=ORIENTED_EDGE('',*,*,#8089,.F.);
#10844=ORIENTED_EDGE('',*,*,#8057,.F.);
#10845=ORIENTED_EDGE('',*,*,#8089,.T.);
#10846=ORIENTED_EDGE('',*,*,#8086,.F.);
#10847=ORIENTED_EDGE('',*,*,#8090,.T.);
#10848=ORIENTED_EDGE('',*,*,#8091,.T.);
#10849=ORIENTED_EDGE('',*,*,#8061,.F.);
#10850=ORIENTED_EDGE('',*,*,#8092,.T.);
#10851=ORIENTED_EDGE('',*,*,#8093,.T.);
#10852=ORIENTED_EDGE('',*,*,#8094,.T.);
#10853=ORIENTED_EDGE('',*,*,#8095,.T.);
#10854=ORIENTED_EDGE('',*,*,#8096,.T.);
#10855=ORIENTED_EDGE('',*,*,#8096,.F.);
#10856=ORIENTED_EDGE('',*,*,#8097,.T.);
#10857=ORIENTED_EDGE('',*,*,#8098,.F.);
#10858=ORIENTED_EDGE('',*,*,#8099,.T.);
#10859=ORIENTED_EDGE('',*,*,#8100,.T.);
#10860=ORIENTED_EDGE('',*,*,#8101,.F.);
#10861=ORIENTED_EDGE('',*,*,#8095,.F.);
#10862=ORIENTED_EDGE('',*,*,#8102,.T.);
#10863=ORIENTED_EDGE('',*,*,#8103,.F.);
#10864=ORIENTED_EDGE('',*,*,#8097,.F.);
#10865=ORIENTED_EDGE('',*,*,#8104,.F.);
#10866=ORIENTED_EDGE('',*,*,#8105,.T.);
#10867=ORIENTED_EDGE('',*,*,#8106,.T.);
#10868=ORIENTED_EDGE('',*,*,#8077,.T.);
#10869=ORIENTED_EDGE('',*,*,#8082,.T.);
#10870=ORIENTED_EDGE('',*,*,#8107,.F.);
#10871=ORIENTED_EDGE('',*,*,#8108,.T.);
#10872=ORIENTED_EDGE('',*,*,#8109,.T.);
#10873=ORIENTED_EDGE('',*,*,#8098,.T.);
#10874=ORIENTED_EDGE('',*,*,#8103,.T.);
#10875=ORIENTED_EDGE('',*,*,#8110,.F.);
#10876=ORIENTED_EDGE('',*,*,#8111,.T.);
#10877=ORIENTED_EDGE('',*,*,#8112,.T.);
#10878=ORIENTED_EDGE('',*,*,#8113,.T.);
#10879=ORIENTED_EDGE('',*,*,#8113,.F.);
#10880=ORIENTED_EDGE('',*,*,#8114,.T.);
#10881=ORIENTED_EDGE('',*,*,#8115,.F.);
#10882=ORIENTED_EDGE('',*,*,#8116,.F.);
#10883=ORIENTED_EDGE('',*,*,#8117,.F.);
#10884=ORIENTED_EDGE('',*,*,#8118,.T.);
#10885=ORIENTED_EDGE('',*,*,#8112,.F.);
#10886=ORIENTED_EDGE('',*,*,#8119,.T.);
#10887=ORIENTED_EDGE('',*,*,#8120,.T.);
#10888=ORIENTED_EDGE('',*,*,#8121,.T.);
#10889=ORIENTED_EDGE('',*,*,#8122,.T.);
#10890=ORIENTED_EDGE('',*,*,#8114,.F.);
#10891=ORIENTED_EDGE('',*,*,#8123,.T.);
#10892=ORIENTED_EDGE('',*,*,#8124,.T.);
#10893=ORIENTED_EDGE('',*,*,#8125,.T.);
#10894=ORIENTED_EDGE('',*,*,#8126,.T.);
#10895=ORIENTED_EDGE('',*,*,#8127,.T.);
#10896=ORIENTED_EDGE('',*,*,#8124,.F.);
#10897=ORIENTED_EDGE('',*,*,#8128,.F.);
#10898=ORIENTED_EDGE('',*,*,#8129,.F.);
#10899=ORIENTED_EDGE('',*,*,#8130,.F.);
#10900=ORIENTED_EDGE('',*,*,#8123,.F.);
#10901=ORIENTED_EDGE('',*,*,#8131,.T.);
#10902=ORIENTED_EDGE('',*,*,#8132,.T.);
#10903=ORIENTED_EDGE('',*,*,#8133,.T.);
#10904=ORIENTED_EDGE('',*,*,#8134,.F.);
#10905=ORIENTED_EDGE('',*,*,#8128,.T.);
#10906=ORIENTED_EDGE('',*,*,#8135,.F.);
#10907=ORIENTED_EDGE('',*,*,#8136,.T.);
#10908=ORIENTED_EDGE('',*,*,#8137,.T.);
#10909=ORIENTED_EDGE('',*,*,#8138,.T.);
#10910=ORIENTED_EDGE('',*,*,#8139,.T.);
#10911=ORIENTED_EDGE('',*,*,#8137,.F.);
#10912=ORIENTED_EDGE('',*,*,#8140,.T.);
#10913=ORIENTED_EDGE('',*,*,#8141,.F.);
#10914=ORIENTED_EDGE('',*,*,#8142,.T.);
#10915=ORIENTED_EDGE('',*,*,#8143,.T.);
#10916=ORIENTED_EDGE('',*,*,#8144,.F.);
#10917=ORIENTED_EDGE('',*,*,#8136,.F.);
#10918=ORIENTED_EDGE('',*,*,#8145,.F.);
#10919=ORIENTED_EDGE('',*,*,#8146,.F.);
#10920=ORIENTED_EDGE('',*,*,#8140,.F.);
#10921=ORIENTED_EDGE('',*,*,#8141,.T.);
#10922=ORIENTED_EDGE('',*,*,#8146,.T.);
#10923=ORIENTED_EDGE('',*,*,#8147,.T.);
#10924=ORIENTED_EDGE('',*,*,#8148,.T.);
#10925=ORIENTED_EDGE('',*,*,#8149,.T.);
#10926=ORIENTED_EDGE('',*,*,#8150,.F.);
#10927=ORIENTED_EDGE('',*,*,#8151,.T.);
#10928=ORIENTED_EDGE('',*,*,#8152,.T.);
#10929=ORIENTED_EDGE('',*,*,#8153,.T.);
#10930=ORIENTED_EDGE('',*,*,#8154,.T.);
#10931=ORIENTED_EDGE('',*,*,#8152,.F.);
#10932=ORIENTED_EDGE('',*,*,#8155,.T.);
#10933=ORIENTED_EDGE('',*,*,#8156,.F.);
#10934=ORIENTED_EDGE('',*,*,#8157,.T.);
#10935=ORIENTED_EDGE('',*,*,#8158,.T.);
#10936=ORIENTED_EDGE('',*,*,#8159,.F.);
#10937=ORIENTED_EDGE('',*,*,#8151,.F.);
#10938=ORIENTED_EDGE('',*,*,#8160,.F.);
#10939=ORIENTED_EDGE('',*,*,#8161,.F.);
#10940=ORIENTED_EDGE('',*,*,#8155,.F.);
#10941=ORIENTED_EDGE('',*,*,#8156,.T.);
#10942=ORIENTED_EDGE('',*,*,#8161,.T.);
#10943=ORIENTED_EDGE('',*,*,#8162,.T.);
#10944=ORIENTED_EDGE('',*,*,#8163,.T.);
#10945=ORIENTED_EDGE('',*,*,#8164,.T.);
#10946=ORIENTED_EDGE('',*,*,#8165,.F.);
#10947=ORIENTED_EDGE('',*,*,#8166,.T.);
#10948=ORIENTED_EDGE('',*,*,#8167,.T.);
#10949=ORIENTED_EDGE('',*,*,#8168,.T.);
#10950=ORIENTED_EDGE('',*,*,#8169,.T.);
#10951=ORIENTED_EDGE('',*,*,#8167,.F.);
#10952=ORIENTED_EDGE('',*,*,#8170,.T.);
#10953=ORIENTED_EDGE('',*,*,#8171,.F.);
#10954=ORIENTED_EDGE('',*,*,#8172,.T.);
#10955=ORIENTED_EDGE('',*,*,#8173,.T.);
#10956=ORIENTED_EDGE('',*,*,#8174,.F.);
#10957=ORIENTED_EDGE('',*,*,#8166,.F.);
#10958=ORIENTED_EDGE('',*,*,#8175,.F.);
#10959=ORIENTED_EDGE('',*,*,#8176,.F.);
#10960=ORIENTED_EDGE('',*,*,#8170,.F.);
#10961=ORIENTED_EDGE('',*,*,#8171,.T.);
#10962=ORIENTED_EDGE('',*,*,#8176,.T.);
#10963=ORIENTED_EDGE('',*,*,#8177,.T.);
#10964=ORIENTED_EDGE('',*,*,#8178,.T.);
#10965=ORIENTED_EDGE('',*,*,#8179,.T.);
#10966=ORIENTED_EDGE('',*,*,#8180,.F.);
#10967=ORIENTED_EDGE('',*,*,#8181,.T.);
#10968=ORIENTED_EDGE('',*,*,#8182,.T.);
#10969=ORIENTED_EDGE('',*,*,#8183,.T.);
#10970=ORIENTED_EDGE('',*,*,#8184,.T.);
#10971=ORIENTED_EDGE('',*,*,#8182,.F.);
#10972=ORIENTED_EDGE('',*,*,#8185,.T.);
#10973=ORIENTED_EDGE('',*,*,#8186,.F.);
#10974=ORIENTED_EDGE('',*,*,#8187,.T.);
#10975=ORIENTED_EDGE('',*,*,#8188,.T.);
#10976=ORIENTED_EDGE('',*,*,#8189,.F.);
#10977=ORIENTED_EDGE('',*,*,#8181,.F.);
#10978=ORIENTED_EDGE('',*,*,#8190,.F.);
#10979=ORIENTED_EDGE('',*,*,#8191,.F.);
#10980=ORIENTED_EDGE('',*,*,#8185,.F.);
#10981=ORIENTED_EDGE('',*,*,#8186,.T.);
#10982=ORIENTED_EDGE('',*,*,#8191,.T.);
#10983=ORIENTED_EDGE('',*,*,#8192,.T.);
#10984=ORIENTED_EDGE('',*,*,#8193,.T.);
#10985=ORIENTED_EDGE('',*,*,#8194,.T.);
#10986=ORIENTED_EDGE('',*,*,#8195,.F.);
#10987=ORIENTED_EDGE('',*,*,#8196,.T.);
#10988=ORIENTED_EDGE('',*,*,#8197,.T.);
#10989=ORIENTED_EDGE('',*,*,#8198,.T.);
#10990=ORIENTED_EDGE('',*,*,#8199,.T.);
#10991=ORIENTED_EDGE('',*,*,#8197,.F.);
#10992=ORIENTED_EDGE('',*,*,#8200,.T.);
#10993=ORIENTED_EDGE('',*,*,#8201,.F.);
#10994=ORIENTED_EDGE('',*,*,#8202,.T.);
#10995=ORIENTED_EDGE('',*,*,#8203,.T.);
#10996=ORIENTED_EDGE('',*,*,#8204,.F.);
#10997=ORIENTED_EDGE('',*,*,#8196,.F.);
#10998=ORIENTED_EDGE('',*,*,#8205,.F.);
#10999=ORIENTED_EDGE('',*,*,#8206,.F.);
#11000=ORIENTED_EDGE('',*,*,#8200,.F.);
#11001=ORIENTED_EDGE('',*,*,#8201,.T.);
#11002=ORIENTED_EDGE('',*,*,#8206,.T.);
#11003=ORIENTED_EDGE('',*,*,#8207,.T.);
#11004=ORIENTED_EDGE('',*,*,#8208,.T.);
#11005=ORIENTED_EDGE('',*,*,#8209,.T.);
#11006=ORIENTED_EDGE('',*,*,#8210,.F.);
#11007=ORIENTED_EDGE('',*,*,#8211,.T.);
#11008=ORIENTED_EDGE('',*,*,#8212,.T.);
#11009=ORIENTED_EDGE('',*,*,#8213,.T.);
#11010=ORIENTED_EDGE('',*,*,#8214,.T.);
#11011=ORIENTED_EDGE('',*,*,#8212,.F.);
#11012=ORIENTED_EDGE('',*,*,#8215,.T.);
#11013=ORIENTED_EDGE('',*,*,#8216,.F.);
#11014=ORIENTED_EDGE('',*,*,#8217,.T.);
#11015=ORIENTED_EDGE('',*,*,#8218,.T.);
#11016=ORIENTED_EDGE('',*,*,#8219,.F.);
#11017=ORIENTED_EDGE('',*,*,#8211,.F.);
#11018=ORIENTED_EDGE('',*,*,#8220,.F.);
#11019=ORIENTED_EDGE('',*,*,#8221,.F.);
#11020=ORIENTED_EDGE('',*,*,#8215,.F.);
#11021=ORIENTED_EDGE('',*,*,#8216,.T.);
#11022=ORIENTED_EDGE('',*,*,#8221,.T.);
#11023=ORIENTED_EDGE('',*,*,#8222,.T.);
#11024=ORIENTED_EDGE('',*,*,#8223,.T.);
#11025=ORIENTED_EDGE('',*,*,#8224,.T.);
#11026=ORIENTED_EDGE('',*,*,#8225,.F.);
#11027=ORIENTED_EDGE('',*,*,#8226,.T.);
#11028=ORIENTED_EDGE('',*,*,#8227,.T.);
#11029=ORIENTED_EDGE('',*,*,#8228,.T.);
#11030=ORIENTED_EDGE('',*,*,#8229,.T.);
#11031=ORIENTED_EDGE('',*,*,#8227,.F.);
#11032=ORIENTED_EDGE('',*,*,#8230,.T.);
#11033=ORIENTED_EDGE('',*,*,#8231,.F.);
#11034=ORIENTED_EDGE('',*,*,#8232,.T.);
#11035=ORIENTED_EDGE('',*,*,#8233,.T.);
#11036=ORIENTED_EDGE('',*,*,#8234,.F.);
#11037=ORIENTED_EDGE('',*,*,#8226,.F.);
#11038=ORIENTED_EDGE('',*,*,#8235,.F.);
#11039=ORIENTED_EDGE('',*,*,#8236,.F.);
#11040=ORIENTED_EDGE('',*,*,#8230,.F.);
#11041=ORIENTED_EDGE('',*,*,#8231,.T.);
#11042=ORIENTED_EDGE('',*,*,#8236,.T.);
#11043=ORIENTED_EDGE('',*,*,#8237,.T.);
#11044=ORIENTED_EDGE('',*,*,#8238,.T.);
#11045=ORIENTED_EDGE('',*,*,#8239,.T.);
#11046=ORIENTED_EDGE('',*,*,#8240,.F.);
#11047=ORIENTED_EDGE('',*,*,#8241,.T.);
#11048=ORIENTED_EDGE('',*,*,#8242,.T.);
#11049=ORIENTED_EDGE('',*,*,#8243,.T.);
#11050=ORIENTED_EDGE('',*,*,#8244,.T.);
#11051=ORIENTED_EDGE('',*,*,#8242,.F.);
#11052=ORIENTED_EDGE('',*,*,#8245,.T.);
#11053=ORIENTED_EDGE('',*,*,#8246,.F.);
#11054=ORIENTED_EDGE('',*,*,#8247,.T.);
#11055=ORIENTED_EDGE('',*,*,#8248,.T.);
#11056=ORIENTED_EDGE('',*,*,#8249,.F.);
#11057=ORIENTED_EDGE('',*,*,#8241,.F.);
#11058=ORIENTED_EDGE('',*,*,#8250,.F.);
#11059=ORIENTED_EDGE('',*,*,#8251,.F.);
#11060=ORIENTED_EDGE('',*,*,#8245,.F.);
#11061=ORIENTED_EDGE('',*,*,#8246,.T.);
#11062=ORIENTED_EDGE('',*,*,#8251,.T.);
#11063=ORIENTED_EDGE('',*,*,#8252,.T.);
#11064=ORIENTED_EDGE('',*,*,#8253,.T.);
#11065=ORIENTED_EDGE('',*,*,#8254,.T.);
#11066=ORIENTED_EDGE('',*,*,#8254,.F.);
#11067=ORIENTED_EDGE('',*,*,#8255,.T.);
#11068=ORIENTED_EDGE('',*,*,#8256,.F.);
#11069=ORIENTED_EDGE('',*,*,#8257,.F.);
#11070=ORIENTED_EDGE('',*,*,#8258,.T.);
#11071=ORIENTED_EDGE('',*,*,#8247,.F.);
#11072=ORIENTED_EDGE('',*,*,#8071,.F.);
#11073=ORIENTED_EDGE('',*,*,#8080,.T.);
#11074=ORIENTED_EDGE('',*,*,#8259,.T.);
#11075=ORIENTED_EDGE('',*,*,#8090,.F.);
#11076=ORIENTED_EDGE('',*,*,#8085,.F.);
#11077=ORIENTED_EDGE('',*,*,#8260,.T.);
#11078=ORIENTED_EDGE('',*,*,#8092,.F.);
#11079=ORIENTED_EDGE('',*,*,#8101,.T.);
#11080=ORIENTED_EDGE('',*,*,#8261,.T.);
#11081=ORIENTED_EDGE('',*,*,#8078,.F.);
#11082=ORIENTED_EDGE('',*,*,#8106,.F.);
#11083=ORIENTED_EDGE('',*,*,#8262,.T.);
#11084=ORIENTED_EDGE('',*,*,#8109,.F.);
#11085=ORIENTED_EDGE('',*,*,#8263,.T.);
#11086=ORIENTED_EDGE('',*,*,#8264,.T.);
#11087=ORIENTED_EDGE('',*,*,#8265,.F.);
#11088=ORIENTED_EDGE('',*,*,#8266,.T.);
#11089=ORIENTED_EDGE('',*,*,#8099,.F.);
#11090=ORIENTED_EDGE('',*,*,#8062,.F.);
#11091=ORIENTED_EDGE('',*,*,#8091,.F.);
#11092=ORIENTED_EDGE('',*,*,#8259,.F.);
#11093=ORIENTED_EDGE('',*,*,#8079,.F.);
#11094=ORIENTED_EDGE('',*,*,#8261,.F.);
#11095=ORIENTED_EDGE('',*,*,#8100,.F.);
#11096=ORIENTED_EDGE('',*,*,#8266,.F.);
#11097=ORIENTED_EDGE('',*,*,#8267,.T.);
#11098=ORIENTED_EDGE('',*,*,#8268,.F.);
#11099=ORIENTED_EDGE('',*,*,#8269,.T.);
#11100=ORIENTED_EDGE('',*,*,#8270,.F.);
#11101=ORIENTED_EDGE('',*,*,#8271,.T.);
#11102=ORIENTED_EDGE('',*,*,#8272,.F.);
#11103=ORIENTED_EDGE('',*,*,#8273,.T.);
#11104=ORIENTED_EDGE('',*,*,#8274,.F.);
#11105=ORIENTED_EDGE('',*,*,#8275,.T.);
#11106=ORIENTED_EDGE('',*,*,#8276,.F.);
#11107=ORIENTED_EDGE('',*,*,#8277,.T.);
#11108=ORIENTED_EDGE('',*,*,#8278,.F.);
#11109=ORIENTED_EDGE('',*,*,#8115,.T.);
#11110=ORIENTED_EDGE('',*,*,#8122,.F.);
#11111=ORIENTED_EDGE('',*,*,#8279,.T.);
#11112=ORIENTED_EDGE('',*,*,#8132,.F.);
#11113=ORIENTED_EDGE('',*,*,#8280,.F.);
#11114=ORIENTED_EDGE('',*,*,#8143,.F.);
#11115=ORIENTED_EDGE('',*,*,#8281,.F.);
#11116=ORIENTED_EDGE('',*,*,#8158,.F.);
#11117=ORIENTED_EDGE('',*,*,#8282,.F.);
#11118=ORIENTED_EDGE('',*,*,#8173,.F.);
#11119=ORIENTED_EDGE('',*,*,#8283,.F.);
#11120=ORIENTED_EDGE('',*,*,#8188,.F.);
#11121=ORIENTED_EDGE('',*,*,#8284,.F.);
#11122=ORIENTED_EDGE('',*,*,#8203,.F.);
#11123=ORIENTED_EDGE('',*,*,#8285,.F.);
#11124=ORIENTED_EDGE('',*,*,#8218,.F.);
#11125=ORIENTED_EDGE('',*,*,#8286,.F.);
#11126=ORIENTED_EDGE('',*,*,#8233,.F.);
#11127=ORIENTED_EDGE('',*,*,#8287,.F.);
#11128=ORIENTED_EDGE('',*,*,#8248,.F.);
#11129=ORIENTED_EDGE('',*,*,#8258,.F.);
#11130=ORIENTED_EDGE('',*,*,#8288,.F.);
#11131=ORIENTED_EDGE('',*,*,#8289,.F.);
#11132=ORIENTED_EDGE('',*,*,#8290,.F.);
#11133=ORIENTED_EDGE('',*,*,#8291,.F.);
#11134=ORIENTED_EDGE('',*,*,#8292,.F.);
#11135=ORIENTED_EDGE('',*,*,#8293,.F.);
#11136=ORIENTED_EDGE('',*,*,#8294,.F.);
#11137=ORIENTED_EDGE('',*,*,#8295,.F.);
#11138=ORIENTED_EDGE('',*,*,#8296,.F.);
#11139=ORIENTED_EDGE('',*,*,#8297,.F.);
#11140=ORIENTED_EDGE('',*,*,#8298,.F.);
#11141=ORIENTED_EDGE('',*,*,#8299,.F.);
#11142=ORIENTED_EDGE('',*,*,#8300,.F.);
#11143=ORIENTED_EDGE('',*,*,#8301,.F.);
#11144=ORIENTED_EDGE('',*,*,#8302,.F.);
#11145=ORIENTED_EDGE('',*,*,#8303,.F.);
#11146=ORIENTED_EDGE('',*,*,#8304,.F.);
#11147=ORIENTED_EDGE('',*,*,#8305,.F.);
#11148=ORIENTED_EDGE('',*,*,#8050,.F.);
#11149=ORIENTED_EDGE('',*,*,#8306,.T.);
#11150=ORIENTED_EDGE('',*,*,#8307,.F.);
#11151=ORIENTED_EDGE('',*,*,#8308,.T.);
#11152=ORIENTED_EDGE('',*,*,#8309,.F.);
#11153=ORIENTED_EDGE('',*,*,#8310,.F.);
#11154=ORIENTED_EDGE('',*,*,#8311,.F.);
#11155=ORIENTED_EDGE('',*,*,#8312,.F.);
#11156=ORIENTED_EDGE('',*,*,#8313,.F.);
#11157=ORIENTED_EDGE('',*,*,#8314,.F.);
#11158=ORIENTED_EDGE('',*,*,#8315,.F.);
#11159=ORIENTED_EDGE('',*,*,#8316,.F.);
#11160=ORIENTED_EDGE('',*,*,#8317,.F.);
#11161=ORIENTED_EDGE('',*,*,#8318,.F.);
#11162=ORIENTED_EDGE('',*,*,#8319,.F.);
#11163=ORIENTED_EDGE('',*,*,#8320,.F.);
#11164=ORIENTED_EDGE('',*,*,#8321,.F.);
#11165=ORIENTED_EDGE('',*,*,#8322,.F.);
#11166=ORIENTED_EDGE('',*,*,#8323,.F.);
#11167=ORIENTED_EDGE('',*,*,#8324,.F.);
#11168=ORIENTED_EDGE('',*,*,#8325,.F.);
#11169=ORIENTED_EDGE('',*,*,#8326,.T.);
#11170=ORIENTED_EDGE('',*,*,#8327,.F.);
#11171=ORIENTED_EDGE('',*,*,#8328,.F.);
#11172=ORIENTED_EDGE('',*,*,#8329,.F.);
#11173=ORIENTED_EDGE('',*,*,#8330,.T.);
#11174=ORIENTED_EDGE('',*,*,#8331,.F.);
#11175=ORIENTED_EDGE('',*,*,#8332,.F.);
#11176=ORIENTED_EDGE('',*,*,#8333,.F.);
#11177=ORIENTED_EDGE('',*,*,#8334,.F.);
#11178=ORIENTED_EDGE('',*,*,#8335,.F.);
#11179=ORIENTED_EDGE('',*,*,#8336,.F.);
#11180=ORIENTED_EDGE('',*,*,#8337,.F.);
#11181=ORIENTED_EDGE('',*,*,#8338,.F.);
#11182=ORIENTED_EDGE('',*,*,#8339,.F.);
#11183=ORIENTED_EDGE('',*,*,#8340,.F.);
#11184=ORIENTED_EDGE('',*,*,#8341,.F.);
#11185=ORIENTED_EDGE('',*,*,#8342,.F.);
#11186=ORIENTED_EDGE('',*,*,#8343,.F.);
#11187=ORIENTED_EDGE('',*,*,#8344,.F.);
#11188=ORIENTED_EDGE('',*,*,#8345,.F.);
#11189=ORIENTED_EDGE('',*,*,#8346,.T.);
#11190=ORIENTED_EDGE('',*,*,#8347,.F.);
#11191=ORIENTED_EDGE('',*,*,#8348,.F.);
#11192=ORIENTED_EDGE('',*,*,#8349,.F.);
#11193=ORIENTED_EDGE('',*,*,#8350,.F.);
#11194=ORIENTED_EDGE('',*,*,#8351,.F.);
#11195=ORIENTED_EDGE('',*,*,#8352,.T.);
#11196=ORIENTED_EDGE('',*,*,#8353,.F.);
#11197=ORIENTED_EDGE('',*,*,#8354,.F.);
#11198=ORIENTED_EDGE('',*,*,#8355,.F.);
#11199=ORIENTED_EDGE('',*,*,#8356,.F.);
#11200=ORIENTED_EDGE('',*,*,#8357,.F.);
#11201=ORIENTED_EDGE('',*,*,#8358,.F.);
#11202=ORIENTED_EDGE('',*,*,#8359,.F.);
#11203=ORIENTED_EDGE('',*,*,#8360,.F.);
#11204=ORIENTED_EDGE('',*,*,#8361,.F.);
#11205=ORIENTED_EDGE('',*,*,#8362,.F.);
#11206=ORIENTED_EDGE('',*,*,#8363,.F.);
#11207=ORIENTED_EDGE('',*,*,#8364,.F.);
#11208=ORIENTED_EDGE('',*,*,#8365,.F.);
#11209=ORIENTED_EDGE('',*,*,#8366,.T.);
#11210=ORIENTED_EDGE('',*,*,#8367,.F.);
#11211=ORIENTED_EDGE('',*,*,#8368,.F.);
#11212=ORIENTED_EDGE('',*,*,#8369,.F.);
#11213=ORIENTED_EDGE('',*,*,#8370,.F.);
#11214=ORIENTED_EDGE('',*,*,#8371,.F.);
#11215=ORIENTED_EDGE('',*,*,#8372,.F.);
#11216=ORIENTED_EDGE('',*,*,#8373,.F.);
#11217=ORIENTED_EDGE('',*,*,#8374,.T.);
#11218=ORIENTED_EDGE('',*,*,#8375,.F.);
#11219=ORIENTED_EDGE('',*,*,#8376,.F.);
#11220=ORIENTED_EDGE('',*,*,#8377,.F.);
#11221=ORIENTED_EDGE('',*,*,#8378,.F.);
#11222=ORIENTED_EDGE('',*,*,#8379,.F.);
#11223=ORIENTED_EDGE('',*,*,#8380,.F.);
#11224=ORIENTED_EDGE('',*,*,#8381,.F.);
#11225=ORIENTED_EDGE('',*,*,#8382,.F.);
#11226=ORIENTED_EDGE('',*,*,#8383,.F.);
#11227=ORIENTED_EDGE('',*,*,#8384,.F.);
#11228=ORIENTED_EDGE('',*,*,#8385,.F.);
#11229=ORIENTED_EDGE('',*,*,#8386,.T.);
#11230=ORIENTED_EDGE('',*,*,#8387,.F.);
#11231=ORIENTED_EDGE('',*,*,#8388,.F.);
#11232=ORIENTED_EDGE('',*,*,#8389,.F.);
#11233=ORIENTED_EDGE('',*,*,#8390,.F.);
#11234=ORIENTED_EDGE('',*,*,#8391,.F.);
#11235=ORIENTED_EDGE('',*,*,#8392,.F.);
#11236=ORIENTED_EDGE('',*,*,#8393,.F.);
#11237=ORIENTED_EDGE('',*,*,#8394,.F.);
#11238=ORIENTED_EDGE('',*,*,#8395,.F.);
#11239=ORIENTED_EDGE('',*,*,#8396,.T.);
#11240=ORIENTED_EDGE('',*,*,#8397,.F.);
#11241=ORIENTED_EDGE('',*,*,#8398,.F.);
#11242=ORIENTED_EDGE('',*,*,#8399,.F.);
#11243=ORIENTED_EDGE('',*,*,#8400,.F.);
#11244=ORIENTED_EDGE('',*,*,#8401,.F.);
#11245=ORIENTED_EDGE('',*,*,#8402,.F.);
#11246=ORIENTED_EDGE('',*,*,#8403,.F.);
#11247=ORIENTED_EDGE('',*,*,#8404,.F.);
#11248=ORIENTED_EDGE('',*,*,#8405,.F.);
#11249=ORIENTED_EDGE('',*,*,#8406,.T.);
#11250=ORIENTED_EDGE('',*,*,#8407,.F.);
#11251=ORIENTED_EDGE('',*,*,#8408,.F.);
#11252=ORIENTED_EDGE('',*,*,#8409,.F.);
#11253=ORIENTED_EDGE('',*,*,#8410,.F.);
#11254=ORIENTED_EDGE('',*,*,#8411,.F.);
#11255=ORIENTED_EDGE('',*,*,#8412,.F.);
#11256=ORIENTED_EDGE('',*,*,#8413,.F.);
#11257=ORIENTED_EDGE('',*,*,#8414,.F.);
#11258=ORIENTED_EDGE('',*,*,#8415,.F.);
#11259=ORIENTED_EDGE('',*,*,#8416,.F.);
#11260=ORIENTED_EDGE('',*,*,#8417,.F.);
#11261=ORIENTED_EDGE('',*,*,#8418,.T.);
#11262=ORIENTED_EDGE('',*,*,#8419,.F.);
#11263=ORIENTED_EDGE('',*,*,#8420,.F.);
#11264=ORIENTED_EDGE('',*,*,#8421,.F.);
#11265=ORIENTED_EDGE('',*,*,#8422,.F.);
#11266=ORIENTED_EDGE('',*,*,#8423,.F.);
#11267=ORIENTED_EDGE('',*,*,#8424,.F.);
#11268=ORIENTED_EDGE('',*,*,#8425,.F.);
#11269=ORIENTED_EDGE('',*,*,#8067,.T.);
#11270=ORIENTED_EDGE('',*,*,#8426,.F.);
#11271=ORIENTED_EDGE('',*,*,#8265,.T.);
#11272=ORIENTED_EDGE('',*,*,#8427,.F.);
#11273=ORIENTED_EDGE('',*,*,#8428,.T.);
#11274=ORIENTED_EDGE('',*,*,#8429,.F.);
#11275=ORIENTED_EDGE('',*,*,#8430,.F.);
#11276=ORIENTED_EDGE('',*,*,#8267,.F.);
#11277=ORIENTED_EDGE('',*,*,#8264,.F.);
#11278=ORIENTED_EDGE('',*,*,#8431,.T.);
#11279=ORIENTED_EDGE('',*,*,#8432,.T.);
#11280=ORIENTED_EDGE('',*,*,#8427,.T.);
#11281=ORIENTED_EDGE('',*,*,#8433,.T.);
#11282=ORIENTED_EDGE('',*,*,#8434,.T.);
#11283=ORIENTED_EDGE('',*,*,#8435,.T.);
#11284=ORIENTED_EDGE('',*,*,#8436,.T.);
#11285=ORIENTED_EDGE('',*,*,#8437,.T.);
#11286=ORIENTED_EDGE('',*,*,#8437,.F.);
#11287=ORIENTED_EDGE('',*,*,#8438,.T.);
#11288=ORIENTED_EDGE('',*,*,#8439,.F.);
#11289=ORIENTED_EDGE('',*,*,#8440,.T.);
#11290=ORIENTED_EDGE('',*,*,#8420,.T.);
#11291=ORIENTED_EDGE('',*,*,#8441,.F.);
#11292=ORIENTED_EDGE('',*,*,#8436,.F.);
#11293=ORIENTED_EDGE('',*,*,#8442,.T.);
#11294=ORIENTED_EDGE('',*,*,#8443,.F.);
#11295=ORIENTED_EDGE('',*,*,#8438,.F.);
#11296=ORIENTED_EDGE('',*,*,#8444,.F.);
#11297=ORIENTED_EDGE('',*,*,#8445,.T.);
#11298=ORIENTED_EDGE('',*,*,#8446,.T.);
#11299=ORIENTED_EDGE('',*,*,#8439,.T.);
#11300=ORIENTED_EDGE('',*,*,#8443,.T.);
#11301=ORIENTED_EDGE('',*,*,#8447,.T.);
#11302=ORIENTED_EDGE('',*,*,#8448,.T.);
#11303=ORIENTED_EDGE('',*,*,#8449,.T.);
#11304=ORIENTED_EDGE('',*,*,#8450,.T.);
#11305=ORIENTED_EDGE('',*,*,#8451,.T.);
#11306=ORIENTED_EDGE('',*,*,#8451,.F.);
#11307=ORIENTED_EDGE('',*,*,#8452,.T.);
#11308=ORIENTED_EDGE('',*,*,#8453,.F.);
#11309=ORIENTED_EDGE('',*,*,#8454,.T.);
#11310=ORIENTED_EDGE('',*,*,#8422,.T.);
#11311=ORIENTED_EDGE('',*,*,#8455,.F.);
#11312=ORIENTED_EDGE('',*,*,#8450,.F.);
#11313=ORIENTED_EDGE('',*,*,#8456,.T.);
#11314=ORIENTED_EDGE('',*,*,#8457,.F.);
#11315=ORIENTED_EDGE('',*,*,#8452,.F.);
#11316=ORIENTED_EDGE('',*,*,#8458,.F.);
#11317=ORIENTED_EDGE('',*,*,#8459,.T.);
#11318=ORIENTED_EDGE('',*,*,#8460,.T.);
#11319=ORIENTED_EDGE('',*,*,#8453,.T.);
#11320=ORIENTED_EDGE('',*,*,#8457,.T.);
#11321=ORIENTED_EDGE('',*,*,#8461,.T.);
#11322=ORIENTED_EDGE('',*,*,#8462,.T.);
#11323=ORIENTED_EDGE('',*,*,#8463,.T.);
#11324=ORIENTED_EDGE('',*,*,#8464,.T.);
#11325=ORIENTED_EDGE('',*,*,#8465,.T.);
#11326=ORIENTED_EDGE('',*,*,#8465,.F.);
#11327=ORIENTED_EDGE('',*,*,#8466,.T.);
#11328=ORIENTED_EDGE('',*,*,#8467,.F.);
#11329=ORIENTED_EDGE('',*,*,#8468,.T.);
#11330=ORIENTED_EDGE('',*,*,#8424,.T.);
#11331=ORIENTED_EDGE('',*,*,#8469,.F.);
#11332=ORIENTED_EDGE('',*,*,#8464,.F.);
#11333=ORIENTED_EDGE('',*,*,#8470,.T.);
#11334=ORIENTED_EDGE('',*,*,#8471,.F.);
#11335=ORIENTED_EDGE('',*,*,#8466,.F.);
#11336=ORIENTED_EDGE('',*,*,#8472,.T.);
#11337=ORIENTED_EDGE('',*,*,#8473,.T.);
#11338=ORIENTED_EDGE('',*,*,#8474,.T.);
#11339=ORIENTED_EDGE('',*,*,#8069,.T.);
#11340=ORIENTED_EDGE('',*,*,#8473,.F.);
#11341=ORIENTED_EDGE('',*,*,#8475,.F.);
#11342=ORIENTED_EDGE('',*,*,#8476,.F.);
#11343=ORIENTED_EDGE('',*,*,#8477,.F.);
#11344=ORIENTED_EDGE('',*,*,#8472,.F.);
#11345=ORIENTED_EDGE('',*,*,#8068,.F.);
#11346=ORIENTED_EDGE('',*,*,#8425,.T.);
#11347=ORIENTED_EDGE('',*,*,#8468,.F.);
#11348=ORIENTED_EDGE('',*,*,#8478,.F.);
#11349=ORIENTED_EDGE('',*,*,#8475,.T.);
#11350=ORIENTED_EDGE('',*,*,#8479,.F.);
#11351=ORIENTED_EDGE('',*,*,#8476,.T.);
#11352=ORIENTED_EDGE('',*,*,#8478,.T.);
#11353=ORIENTED_EDGE('',*,*,#8467,.T.);
#11354=ORIENTED_EDGE('',*,*,#8471,.T.);
#11355=ORIENTED_EDGE('',*,*,#8480,.F.);
#11356=ORIENTED_EDGE('',*,*,#8481,.T.);
#11357=ORIENTED_EDGE('',*,*,#8482,.T.);
#11358=ORIENTED_EDGE('',*,*,#8483,.T.);
#11359=ORIENTED_EDGE('',*,*,#8482,.F.);
#11360=ORIENTED_EDGE('',*,*,#8484,.T.);
#11361=ORIENTED_EDGE('',*,*,#8485,.F.);
#11362=ORIENTED_EDGE('',*,*,#8486,.T.);
#11363=ORIENTED_EDGE('',*,*,#8407,.T.);
#11364=ORIENTED_EDGE('',*,*,#8487,.F.);
#11365=ORIENTED_EDGE('',*,*,#8481,.F.);
#11366=ORIENTED_EDGE('',*,*,#8488,.F.);
#11367=ORIENTED_EDGE('',*,*,#8489,.F.);
#11368=ORIENTED_EDGE('',*,*,#8484,.F.);
#11369=ORIENTED_EDGE('',*,*,#8485,.T.);
#11370=ORIENTED_EDGE('',*,*,#8489,.T.);
#11371=ORIENTED_EDGE('',*,*,#8490,.T.);
#11372=ORIENTED_EDGE('',*,*,#8491,.T.);
#11373=ORIENTED_EDGE('',*,*,#8492,.T.);
#11374=ORIENTED_EDGE('',*,*,#8493,.F.);
#11375=ORIENTED_EDGE('',*,*,#8494,.T.);
#11376=ORIENTED_EDGE('',*,*,#8495,.T.);
#11377=ORIENTED_EDGE('',*,*,#8496,.T.);
#11378=ORIENTED_EDGE('',*,*,#8497,.T.);
#11379=ORIENTED_EDGE('',*,*,#8495,.F.);
#11380=ORIENTED_EDGE('',*,*,#8498,.T.);
#11381=ORIENTED_EDGE('',*,*,#8499,.F.);
#11382=ORIENTED_EDGE('',*,*,#8500,.T.);
#11383=ORIENTED_EDGE('',*,*,#8409,.T.);
#11384=ORIENTED_EDGE('',*,*,#8501,.F.);
#11385=ORIENTED_EDGE('',*,*,#8494,.F.);
#11386=ORIENTED_EDGE('',*,*,#8502,.F.);
#11387=ORIENTED_EDGE('',*,*,#8503,.F.);
#11388=ORIENTED_EDGE('',*,*,#8498,.F.);
#11389=ORIENTED_EDGE('',*,*,#8499,.T.);
#11390=ORIENTED_EDGE('',*,*,#8503,.T.);
#11391=ORIENTED_EDGE('',*,*,#8504,.T.);
#11392=ORIENTED_EDGE('',*,*,#8505,.T.);
#11393=ORIENTED_EDGE('',*,*,#8506,.T.);
#11394=ORIENTED_EDGE('',*,*,#8507,.F.);
#11395=ORIENTED_EDGE('',*,*,#8508,.T.);
#11396=ORIENTED_EDGE('',*,*,#8509,.T.);
#11397=ORIENTED_EDGE('',*,*,#8510,.T.);
#11398=ORIENTED_EDGE('',*,*,#8511,.T.);
#11399=ORIENTED_EDGE('',*,*,#8509,.F.);
#11400=ORIENTED_EDGE('',*,*,#8512,.T.);
#11401=ORIENTED_EDGE('',*,*,#8513,.F.);
#11402=ORIENTED_EDGE('',*,*,#8514,.T.);
#11403=ORIENTED_EDGE('',*,*,#8411,.T.);
#11404=ORIENTED_EDGE('',*,*,#8515,.F.);
#11405=ORIENTED_EDGE('',*,*,#8508,.F.);
#11406=ORIENTED_EDGE('',*,*,#8516,.F.);
#11407=ORIENTED_EDGE('',*,*,#8517,.F.);
#11408=ORIENTED_EDGE('',*,*,#8512,.F.);
#11409=ORIENTED_EDGE('',*,*,#8513,.T.);
#11410=ORIENTED_EDGE('',*,*,#8517,.T.);
#11411=ORIENTED_EDGE('',*,*,#8518,.T.);
#11412=ORIENTED_EDGE('',*,*,#8519,.T.);
#11413=ORIENTED_EDGE('',*,*,#8520,.T.);
#11414=ORIENTED_EDGE('',*,*,#8521,.F.);
#11415=ORIENTED_EDGE('',*,*,#8522,.T.);
#11416=ORIENTED_EDGE('',*,*,#8523,.T.);
#11417=ORIENTED_EDGE('',*,*,#8524,.T.);
#11418=ORIENTED_EDGE('',*,*,#8525,.T.);
#11419=ORIENTED_EDGE('',*,*,#8523,.F.);
#11420=ORIENTED_EDGE('',*,*,#8526,.T.);
#11421=ORIENTED_EDGE('',*,*,#8527,.F.);
#11422=ORIENTED_EDGE('',*,*,#8528,.T.);
#11423=ORIENTED_EDGE('',*,*,#8413,.T.);
#11424=ORIENTED_EDGE('',*,*,#8529,.F.);
#11425=ORIENTED_EDGE('',*,*,#8522,.F.);
#11426=ORIENTED_EDGE('',*,*,#8530,.F.);
#11427=ORIENTED_EDGE('',*,*,#8531,.F.);
#11428=ORIENTED_EDGE('',*,*,#8526,.F.);
#11429=ORIENTED_EDGE('',*,*,#8527,.T.);
#11430=ORIENTED_EDGE('',*,*,#8531,.T.);
#11431=ORIENTED_EDGE('',*,*,#8532,.T.);
#11432=ORIENTED_EDGE('',*,*,#8533,.T.);
#11433=ORIENTED_EDGE('',*,*,#8534,.T.);
#11434=ORIENTED_EDGE('',*,*,#8535,.F.);
#11435=ORIENTED_EDGE('',*,*,#8536,.T.);
#11436=ORIENTED_EDGE('',*,*,#8537,.T.);
#11437=ORIENTED_EDGE('',*,*,#8538,.T.);
#11438=ORIENTED_EDGE('',*,*,#8539,.T.);
#11439=ORIENTED_EDGE('',*,*,#8537,.F.);
#11440=ORIENTED_EDGE('',*,*,#8540,.T.);
#11441=ORIENTED_EDGE('',*,*,#8541,.F.);
#11442=ORIENTED_EDGE('',*,*,#8542,.T.);
#11443=ORIENTED_EDGE('',*,*,#8415,.T.);
#11444=ORIENTED_EDGE('',*,*,#8543,.F.);
#11445=ORIENTED_EDGE('',*,*,#8536,.F.);
#11446=ORIENTED_EDGE('',*,*,#8544,.F.);
#11447=ORIENTED_EDGE('',*,*,#8545,.F.);
#11448=ORIENTED_EDGE('',*,*,#8540,.F.);
#11449=ORIENTED_EDGE('',*,*,#8541,.T.);
#11450=ORIENTED_EDGE('',*,*,#8545,.T.);
#11451=ORIENTED_EDGE('',*,*,#8546,.T.);
#11452=ORIENTED_EDGE('',*,*,#8547,.T.);
#11453=ORIENTED_EDGE('',*,*,#8548,.T.);
#11454=ORIENTED_EDGE('',*,*,#8549,.F.);
#11455=ORIENTED_EDGE('',*,*,#8550,.T.);
#11456=ORIENTED_EDGE('',*,*,#8551,.T.);
#11457=ORIENTED_EDGE('',*,*,#8552,.T.);
#11458=ORIENTED_EDGE('',*,*,#8553,.T.);
#11459=ORIENTED_EDGE('',*,*,#8551,.F.);
#11460=ORIENTED_EDGE('',*,*,#8554,.T.);
#11461=ORIENTED_EDGE('',*,*,#8555,.F.);
#11462=ORIENTED_EDGE('',*,*,#8556,.F.);
#11463=ORIENTED_EDGE('',*,*,#8417,.T.);
#11464=ORIENTED_EDGE('',*,*,#8557,.F.);
#11465=ORIENTED_EDGE('',*,*,#8550,.F.);
#11466=ORIENTED_EDGE('',*,*,#8558,.F.);
#11467=ORIENTED_EDGE('',*,*,#8559,.F.);
#11468=ORIENTED_EDGE('',*,*,#8554,.F.);
#11469=ORIENTED_EDGE('',*,*,#8560,.T.);
#11470=ORIENTED_EDGE('',*,*,#8561,.F.);
#11471=ORIENTED_EDGE('',*,*,#8562,.T.);
#11472=ORIENTED_EDGE('',*,*,#8563,.T.);
#11473=ORIENTED_EDGE('',*,*,#8433,.F.);
#11474=ORIENTED_EDGE('',*,*,#8441,.T.);
#11475=ORIENTED_EDGE('',*,*,#8419,.T.);
#11476=ORIENTED_EDGE('',*,*,#8564,.T.);
#11477=ORIENTED_EDGE('',*,*,#8563,.F.);
#11478=ORIENTED_EDGE('',*,*,#8565,.T.);
#11479=ORIENTED_EDGE('',*,*,#8446,.F.);
#11480=ORIENTED_EDGE('',*,*,#8566,.T.);
#11481=ORIENTED_EDGE('',*,*,#8447,.F.);
#11482=ORIENTED_EDGE('',*,*,#8455,.T.);
#11483=ORIENTED_EDGE('',*,*,#8421,.T.);
#11484=ORIENTED_EDGE('',*,*,#8440,.F.);
#11485=ORIENTED_EDGE('',*,*,#8460,.F.);
#11486=ORIENTED_EDGE('',*,*,#8567,.T.);
#11487=ORIENTED_EDGE('',*,*,#8461,.F.);
#11488=ORIENTED_EDGE('',*,*,#8469,.T.);
#11489=ORIENTED_EDGE('',*,*,#8423,.T.);
#11490=ORIENTED_EDGE('',*,*,#8454,.F.);
#11491=ORIENTED_EDGE('',*,*,#8459,.F.);
#11492=ORIENTED_EDGE('',*,*,#8568,.F.);
#11493=ORIENTED_EDGE('',*,*,#8462,.F.);
#11494=ORIENTED_EDGE('',*,*,#8567,.F.);
#11495=ORIENTED_EDGE('',*,*,#8445,.F.);
#11496=ORIENTED_EDGE('',*,*,#8569,.F.);
#11497=ORIENTED_EDGE('',*,*,#8448,.F.);
#11498=ORIENTED_EDGE('',*,*,#8566,.F.);
#11499=ORIENTED_EDGE('',*,*,#8434,.F.);
#11500=ORIENTED_EDGE('',*,*,#8565,.F.);
#11501=ORIENTED_EDGE('',*,*,#8562,.F.);
#11502=ORIENTED_EDGE('',*,*,#8570,.F.);
#11503=ORIENTED_EDGE('',*,*,#8555,.T.);
#11504=ORIENTED_EDGE('',*,*,#8559,.T.);
#11505=ORIENTED_EDGE('',*,*,#8571,.T.);
#11506=ORIENTED_EDGE('',*,*,#8572,.T.);
#11507=ORIENTED_EDGE('',*,*,#8492,.F.);
#11508=ORIENTED_EDGE('',*,*,#8573,.T.);
#11509=ORIENTED_EDGE('',*,*,#8496,.F.);
#11510=ORIENTED_EDGE('',*,*,#8501,.T.);
#11511=ORIENTED_EDGE('',*,*,#8408,.T.);
#11512=ORIENTED_EDGE('',*,*,#8486,.F.);
#11513=ORIENTED_EDGE('',*,*,#8506,.F.);
#11514=ORIENTED_EDGE('',*,*,#8574,.T.);
#11515=ORIENTED_EDGE('',*,*,#8510,.F.);
#11516=ORIENTED_EDGE('',*,*,#8515,.T.);
#11517=ORIENTED_EDGE('',*,*,#8410,.T.);
#11518=ORIENTED_EDGE('',*,*,#8500,.F.);
#11519=ORIENTED_EDGE('',*,*,#8520,.F.);
#11520=ORIENTED_EDGE('',*,*,#8575,.T.);
#11521=ORIENTED_EDGE('',*,*,#8524,.F.);
#11522=ORIENTED_EDGE('',*,*,#8529,.T.);
#11523=ORIENTED_EDGE('',*,*,#8412,.T.);
#11524=ORIENTED_EDGE('',*,*,#8514,.F.);
#11525=ORIENTED_EDGE('',*,*,#8534,.F.);
#11526=ORIENTED_EDGE('',*,*,#8576,.T.);
#11527=ORIENTED_EDGE('',*,*,#8538,.F.);
#11528=ORIENTED_EDGE('',*,*,#8543,.T.);
#11529=ORIENTED_EDGE('',*,*,#8414,.T.);
#11530=ORIENTED_EDGE('',*,*,#8528,.F.);
#11531=ORIENTED_EDGE('',*,*,#8548,.F.);
#11532=ORIENTED_EDGE('',*,*,#8577,.T.);
#11533=ORIENTED_EDGE('',*,*,#8552,.F.);
#11534=ORIENTED_EDGE('',*,*,#8557,.T.);
#11535=ORIENTED_EDGE('',*,*,#8416,.T.);
#11536=ORIENTED_EDGE('',*,*,#8542,.F.);
#11537=ORIENTED_EDGE('',*,*,#8564,.F.);
#11538=ORIENTED_EDGE('',*,*,#8418,.F.);
#11539=ORIENTED_EDGE('',*,*,#8556,.T.);
#11540=ORIENTED_EDGE('',*,*,#8572,.F.);
#11541=ORIENTED_EDGE('',*,*,#8578,.T.);
#11542=ORIENTED_EDGE('',*,*,#8560,.F.);
#11543=ORIENTED_EDGE('',*,*,#8547,.F.);
#11544=ORIENTED_EDGE('',*,*,#8579,.T.);
#11545=ORIENTED_EDGE('',*,*,#8553,.F.);
#11546=ORIENTED_EDGE('',*,*,#8577,.F.);
#11547=ORIENTED_EDGE('',*,*,#8533,.F.);
#11548=ORIENTED_EDGE('',*,*,#8580,.T.);
#11549=ORIENTED_EDGE('',*,*,#8539,.F.);
#11550=ORIENTED_EDGE('',*,*,#8576,.F.);
#11551=ORIENTED_EDGE('',*,*,#8519,.F.);
#11552=ORIENTED_EDGE('',*,*,#8581,.T.);
#11553=ORIENTED_EDGE('',*,*,#8525,.F.);
#11554=ORIENTED_EDGE('',*,*,#8575,.F.);
#11555=ORIENTED_EDGE('',*,*,#8505,.F.);
#11556=ORIENTED_EDGE('',*,*,#8582,.T.);
#11557=ORIENTED_EDGE('',*,*,#8511,.F.);
#11558=ORIENTED_EDGE('',*,*,#8574,.F.);
#11559=ORIENTED_EDGE('',*,*,#8491,.F.);
#11560=ORIENTED_EDGE('',*,*,#8583,.T.);
#11561=ORIENTED_EDGE('',*,*,#8497,.F.);
#11562=ORIENTED_EDGE('',*,*,#8573,.F.);
#11563=ORIENTED_EDGE('',*,*,#8584,.T.);
#11564=ORIENTED_EDGE('',*,*,#8585,.T.);
#11565=ORIENTED_EDGE('',*,*,#8586,.T.);
#11566=ORIENTED_EDGE('',*,*,#8587,.T.);
#11567=ORIENTED_EDGE('',*,*,#8588,.T.);
#11568=ORIENTED_EDGE('',*,*,#8588,.F.);
#11569=ORIENTED_EDGE('',*,*,#8589,.T.);
#11570=ORIENTED_EDGE('',*,*,#8590,.F.);
#11571=ORIENTED_EDGE('',*,*,#8591,.F.);
#11572=ORIENTED_EDGE('',*,*,#8398,.T.);
#11573=ORIENTED_EDGE('',*,*,#8592,.F.);
#11574=ORIENTED_EDGE('',*,*,#8587,.F.);
#11575=ORIENTED_EDGE('',*,*,#8593,.T.);
#11576=ORIENTED_EDGE('',*,*,#8594,.F.);
#11577=ORIENTED_EDGE('',*,*,#8589,.F.);
#11578=ORIENTED_EDGE('',*,*,#8595,.F.);
#11579=ORIENTED_EDGE('',*,*,#8596,.T.);
#11580=ORIENTED_EDGE('',*,*,#8597,.T.);
#11581=ORIENTED_EDGE('',*,*,#8590,.T.);
#11582=ORIENTED_EDGE('',*,*,#8594,.T.);
#11583=ORIENTED_EDGE('',*,*,#8597,.F.);
#11584=ORIENTED_EDGE('',*,*,#8598,.T.);
#11585=ORIENTED_EDGE('',*,*,#8599,.F.);
#11586=ORIENTED_EDGE('',*,*,#8600,.T.);
#11587=ORIENTED_EDGE('',*,*,#8399,.T.);
#11588=ORIENTED_EDGE('',*,*,#8591,.T.);
#11589=ORIENTED_EDGE('',*,*,#8599,.T.);
#11590=ORIENTED_EDGE('',*,*,#8601,.T.);
#11591=ORIENTED_EDGE('',*,*,#8602,.T.);
#11592=ORIENTED_EDGE('',*,*,#8603,.T.);
#11593=ORIENTED_EDGE('',*,*,#8604,.T.);
#11594=ORIENTED_EDGE('',*,*,#8604,.F.);
#11595=ORIENTED_EDGE('',*,*,#8605,.T.);
#11596=ORIENTED_EDGE('',*,*,#8606,.F.);
#11597=ORIENTED_EDGE('',*,*,#8607,.T.);
#11598=ORIENTED_EDGE('',*,*,#8400,.T.);
#11599=ORIENTED_EDGE('',*,*,#8600,.F.);
#11600=ORIENTED_EDGE('',*,*,#8603,.F.);
#11601=ORIENTED_EDGE('',*,*,#8608,.T.);
#11602=ORIENTED_EDGE('',*,*,#8609,.F.);
#11603=ORIENTED_EDGE('',*,*,#8605,.F.);
#11604=ORIENTED_EDGE('',*,*,#8610,.F.);
#11605=ORIENTED_EDGE('',*,*,#8611,.T.);
#11606=ORIENTED_EDGE('',*,*,#8612,.T.);
#11607=ORIENTED_EDGE('',*,*,#8606,.T.);
#11608=ORIENTED_EDGE('',*,*,#8609,.T.);
#11609=ORIENTED_EDGE('',*,*,#8613,.T.);
#11610=ORIENTED_EDGE('',*,*,#8614,.T.);
#11611=ORIENTED_EDGE('',*,*,#8615,.T.);
#11612=ORIENTED_EDGE('',*,*,#8616,.T.);
#11613=ORIENTED_EDGE('',*,*,#8617,.T.);
#11614=ORIENTED_EDGE('',*,*,#8617,.F.);
#11615=ORIENTED_EDGE('',*,*,#8618,.T.);
#11616=ORIENTED_EDGE('',*,*,#8619,.F.);
#11617=ORIENTED_EDGE('',*,*,#8620,.T.);
#11618=ORIENTED_EDGE('',*,*,#8402,.T.);
#11619=ORIENTED_EDGE('',*,*,#8621,.F.);
#11620=ORIENTED_EDGE('',*,*,#8616,.F.);
#11621=ORIENTED_EDGE('',*,*,#8622,.T.);
#11622=ORIENTED_EDGE('',*,*,#8623,.F.);
#11623=ORIENTED_EDGE('',*,*,#8618,.F.);
#11624=ORIENTED_EDGE('',*,*,#8624,.F.);
#11625=ORIENTED_EDGE('',*,*,#8625,.T.);
#11626=ORIENTED_EDGE('',*,*,#8626,.T.);
#11627=ORIENTED_EDGE('',*,*,#8619,.T.);
#11628=ORIENTED_EDGE('',*,*,#8623,.T.);
#11629=ORIENTED_EDGE('',*,*,#8627,.T.);
#11630=ORIENTED_EDGE('',*,*,#8628,.T.);
#11631=ORIENTED_EDGE('',*,*,#8629,.T.);
#11632=ORIENTED_EDGE('',*,*,#8630,.T.);
#11633=ORIENTED_EDGE('',*,*,#8631,.T.);
#11634=ORIENTED_EDGE('',*,*,#8631,.F.);
#11635=ORIENTED_EDGE('',*,*,#8632,.T.);
#11636=ORIENTED_EDGE('',*,*,#8633,.F.);
#11637=ORIENTED_EDGE('',*,*,#8634,.T.);
#11638=ORIENTED_EDGE('',*,*,#8404,.T.);
#11639=ORIENTED_EDGE('',*,*,#8635,.F.);
#11640=ORIENTED_EDGE('',*,*,#8630,.F.);
#11641=ORIENTED_EDGE('',*,*,#8636,.T.);
#11642=ORIENTED_EDGE('',*,*,#8637,.F.);
#11643=ORIENTED_EDGE('',*,*,#8632,.F.);
#11644=ORIENTED_EDGE('',*,*,#8638,.T.);
#11645=ORIENTED_EDGE('',*,*,#8639,.T.);
#11646=ORIENTED_EDGE('',*,*,#8640,.T.);
#11647=ORIENTED_EDGE('',*,*,#8641,.T.);
#11648=ORIENTED_EDGE('',*,*,#8639,.F.);
#11649=ORIENTED_EDGE('',*,*,#8642,.F.);
#11650=ORIENTED_EDGE('',*,*,#8643,.F.);
#11651=ORIENTED_EDGE('',*,*,#8644,.F.);
#11652=ORIENTED_EDGE('',*,*,#8638,.F.);
#11653=ORIENTED_EDGE('',*,*,#8645,.F.);
#11654=ORIENTED_EDGE('',*,*,#8405,.T.);
#11655=ORIENTED_EDGE('',*,*,#8634,.F.);
#11656=ORIENTED_EDGE('',*,*,#8646,.F.);
#11657=ORIENTED_EDGE('',*,*,#8642,.T.);
#11658=ORIENTED_EDGE('',*,*,#8647,.F.);
#11659=ORIENTED_EDGE('',*,*,#8643,.T.);
#11660=ORIENTED_EDGE('',*,*,#8646,.T.);
#11661=ORIENTED_EDGE('',*,*,#8633,.T.);
#11662=ORIENTED_EDGE('',*,*,#8637,.T.);
#11663=ORIENTED_EDGE('',*,*,#8648,.F.);
#11664=ORIENTED_EDGE('',*,*,#8649,.T.);
#11665=ORIENTED_EDGE('',*,*,#8650,.T.);
#11666=ORIENTED_EDGE('',*,*,#8651,.T.);
#11667=ORIENTED_EDGE('',*,*,#8650,.F.);
#11668=ORIENTED_EDGE('',*,*,#8652,.T.);
#11669=ORIENTED_EDGE('',*,*,#8653,.F.);
#11670=ORIENTED_EDGE('',*,*,#8654,.T.);
#11671=ORIENTED_EDGE('',*,*,#8387,.T.);
#11672=ORIENTED_EDGE('',*,*,#8655,.F.);
#11673=ORIENTED_EDGE('',*,*,#8649,.F.);
#11674=ORIENTED_EDGE('',*,*,#8656,.F.);
#11675=ORIENTED_EDGE('',*,*,#8657,.F.);
#11676=ORIENTED_EDGE('',*,*,#8652,.F.);
#11677=ORIENTED_EDGE('',*,*,#8653,.T.);
#11678=ORIENTED_EDGE('',*,*,#8657,.T.);
#11679=ORIENTED_EDGE('',*,*,#8658,.T.);
#11680=ORIENTED_EDGE('',*,*,#8659,.T.);
#11681=ORIENTED_EDGE('',*,*,#8660,.T.);
#11682=ORIENTED_EDGE('',*,*,#8661,.F.);
#11683=ORIENTED_EDGE('',*,*,#8662,.T.);
#11684=ORIENTED_EDGE('',*,*,#8663,.T.);
#11685=ORIENTED_EDGE('',*,*,#8664,.T.);
#11686=ORIENTED_EDGE('',*,*,#8665,.T.);
#11687=ORIENTED_EDGE('',*,*,#8663,.F.);
#11688=ORIENTED_EDGE('',*,*,#8666,.T.);
#11689=ORIENTED_EDGE('',*,*,#8667,.F.);
#11690=ORIENTED_EDGE('',*,*,#8668,.T.);
#11691=ORIENTED_EDGE('',*,*,#8389,.T.);
#11692=ORIENTED_EDGE('',*,*,#8669,.F.);
#11693=ORIENTED_EDGE('',*,*,#8662,.F.);
#11694=ORIENTED_EDGE('',*,*,#8670,.F.);
#11695=ORIENTED_EDGE('',*,*,#8671,.F.);
#11696=ORIENTED_EDGE('',*,*,#8666,.F.);
#11697=ORIENTED_EDGE('',*,*,#8667,.T.);
#11698=ORIENTED_EDGE('',*,*,#8671,.T.);
#11699=ORIENTED_EDGE('',*,*,#8672,.T.);
#11700=ORIENTED_EDGE('',*,*,#8673,.T.);
#11701=ORIENTED_EDGE('',*,*,#8674,.T.);
#11702=ORIENTED_EDGE('',*,*,#8675,.F.);
#11703=ORIENTED_EDGE('',*,*,#8676,.T.);
#11704=ORIENTED_EDGE('',*,*,#8677,.T.);
#11705=ORIENTED_EDGE('',*,*,#8678,.T.);
#11706=ORIENTED_EDGE('',*,*,#8679,.T.);
#11707=ORIENTED_EDGE('',*,*,#8677,.F.);
#11708=ORIENTED_EDGE('',*,*,#8680,.T.);
#11709=ORIENTED_EDGE('',*,*,#8681,.F.);
#11710=ORIENTED_EDGE('',*,*,#8682,.T.);
#11711=ORIENTED_EDGE('',*,*,#8391,.T.);
#11712=ORIENTED_EDGE('',*,*,#8683,.F.);
#11713=ORIENTED_EDGE('',*,*,#8676,.F.);
#11714=ORIENTED_EDGE('',*,*,#8684,.F.);
#11715=ORIENTED_EDGE('',*,*,#8685,.F.);
#11716=ORIENTED_EDGE('',*,*,#8680,.F.);
#11717=ORIENTED_EDGE('',*,*,#8681,.T.);
#11718=ORIENTED_EDGE('',*,*,#8685,.T.);
#11719=ORIENTED_EDGE('',*,*,#8686,.T.);
#11720=ORIENTED_EDGE('',*,*,#8687,.T.);
#11721=ORIENTED_EDGE('',*,*,#8688,.T.);
#11722=ORIENTED_EDGE('',*,*,#8689,.F.);
#11723=ORIENTED_EDGE('',*,*,#8690,.T.);
#11724=ORIENTED_EDGE('',*,*,#8691,.T.);
#11725=ORIENTED_EDGE('',*,*,#8692,.T.);
#11726=ORIENTED_EDGE('',*,*,#8693,.T.);
#11727=ORIENTED_EDGE('',*,*,#8691,.F.);
#11728=ORIENTED_EDGE('',*,*,#8694,.T.);
#11729=ORIENTED_EDGE('',*,*,#8695,.F.);
#11730=ORIENTED_EDGE('',*,*,#8696,.T.);
#11731=ORIENTED_EDGE('',*,*,#8393,.T.);
#11732=ORIENTED_EDGE('',*,*,#8697,.F.);
#11733=ORIENTED_EDGE('',*,*,#8690,.F.);
#11734=ORIENTED_EDGE('',*,*,#8698,.F.);
#11735=ORIENTED_EDGE('',*,*,#8699,.F.);
#11736=ORIENTED_EDGE('',*,*,#8694,.F.);
#11737=ORIENTED_EDGE('',*,*,#8695,.T.);
#11738=ORIENTED_EDGE('',*,*,#8699,.T.);
#11739=ORIENTED_EDGE('',*,*,#8700,.T.);
#11740=ORIENTED_EDGE('',*,*,#8701,.T.);
#11741=ORIENTED_EDGE('',*,*,#8702,.T.);
#11742=ORIENTED_EDGE('',*,*,#8703,.F.);
#11743=ORIENTED_EDGE('',*,*,#8704,.T.);
#11744=ORIENTED_EDGE('',*,*,#8705,.T.);
#11745=ORIENTED_EDGE('',*,*,#8706,.T.);
#11746=ORIENTED_EDGE('',*,*,#8707,.T.);
#11747=ORIENTED_EDGE('',*,*,#8705,.F.);
#11748=ORIENTED_EDGE('',*,*,#8708,.T.);
#11749=ORIENTED_EDGE('',*,*,#8709,.F.);
#11750=ORIENTED_EDGE('',*,*,#8710,.F.);
#11751=ORIENTED_EDGE('',*,*,#8395,.T.);
#11752=ORIENTED_EDGE('',*,*,#8711,.T.);
#11753=ORIENTED_EDGE('',*,*,#8704,.F.);
#11754=ORIENTED_EDGE('',*,*,#8712,.F.);
#11755=ORIENTED_EDGE('',*,*,#8713,.F.);
#11756=ORIENTED_EDGE('',*,*,#8708,.F.);
#11757=ORIENTED_EDGE('',*,*,#8714,.T.);
#11758=ORIENTED_EDGE('',*,*,#8715,.F.);
#11759=ORIENTED_EDGE('',*,*,#8716,.T.);
#11760=ORIENTED_EDGE('',*,*,#8717,.T.);
#11761=ORIENTED_EDGE('',*,*,#8584,.F.);
#11762=ORIENTED_EDGE('',*,*,#8592,.T.);
#11763=ORIENTED_EDGE('',*,*,#8397,.T.);
#11764=ORIENTED_EDGE('',*,*,#8718,.T.);
#11765=ORIENTED_EDGE('',*,*,#8717,.F.);
#11766=ORIENTED_EDGE('',*,*,#8719,.T.);
#11767=ORIENTED_EDGE('',*,*,#8612,.F.);
#11768=ORIENTED_EDGE('',*,*,#8720,.T.);
#11769=ORIENTED_EDGE('',*,*,#8613,.F.);
#11770=ORIENTED_EDGE('',*,*,#8621,.T.);
#11771=ORIENTED_EDGE('',*,*,#8401,.T.);
#11772=ORIENTED_EDGE('',*,*,#8607,.F.);
#11773=ORIENTED_EDGE('',*,*,#8626,.F.);
#11774=ORIENTED_EDGE('',*,*,#8721,.T.);
#11775=ORIENTED_EDGE('',*,*,#8627,.F.);
#11776=ORIENTED_EDGE('',*,*,#8635,.T.);
#11777=ORIENTED_EDGE('',*,*,#8403,.T.);
#11778=ORIENTED_EDGE('',*,*,#8620,.F.);
#11779=ORIENTED_EDGE('',*,*,#8625,.F.);
#11780=ORIENTED_EDGE('',*,*,#8722,.F.);
#11781=ORIENTED_EDGE('',*,*,#8628,.F.);
#11782=ORIENTED_EDGE('',*,*,#8721,.F.);
#11783=ORIENTED_EDGE('',*,*,#8611,.F.);
#11784=ORIENTED_EDGE('',*,*,#8723,.F.);
#11785=ORIENTED_EDGE('',*,*,#8614,.F.);
#11786=ORIENTED_EDGE('',*,*,#8720,.F.);
#11787=ORIENTED_EDGE('',*,*,#8596,.F.);
#11788=ORIENTED_EDGE('',*,*,#8724,.F.);
#11789=ORIENTED_EDGE('',*,*,#8601,.F.);
#11790=ORIENTED_EDGE('',*,*,#8598,.F.);
#11791=ORIENTED_EDGE('',*,*,#8585,.F.);
#11792=ORIENTED_EDGE('',*,*,#8719,.F.);
#11793=ORIENTED_EDGE('',*,*,#8716,.F.);
#11794=ORIENTED_EDGE('',*,*,#8725,.F.);
#11795=ORIENTED_EDGE('',*,*,#8709,.T.);
#11796=ORIENTED_EDGE('',*,*,#8713,.T.);
#11797=ORIENTED_EDGE('',*,*,#8726,.T.);
#11798=ORIENTED_EDGE('',*,*,#8727,.T.);
#11799=ORIENTED_EDGE('',*,*,#8660,.F.);
#11800=ORIENTED_EDGE('',*,*,#8728,.T.);
#11801=ORIENTED_EDGE('',*,*,#8664,.F.);
#11802=ORIENTED_EDGE('',*,*,#8669,.T.);
#11803=ORIENTED_EDGE('',*,*,#8388,.T.);
#11804=ORIENTED_EDGE('',*,*,#8654,.F.);
#11805=ORIENTED_EDGE('',*,*,#8674,.F.);
#11806=ORIENTED_EDGE('',*,*,#8729,.T.);
#11807=ORIENTED_EDGE('',*,*,#8678,.F.);
#11808=ORIENTED_EDGE('',*,*,#8683,.T.);
#11809=ORIENTED_EDGE('',*,*,#8390,.T.);
#11810=ORIENTED_EDGE('',*,*,#8668,.F.);
#11811=ORIENTED_EDGE('',*,*,#8688,.F.);
#11812=ORIENTED_EDGE('',*,*,#8730,.T.);
#11813=ORIENTED_EDGE('',*,*,#8692,.F.);
#11814=ORIENTED_EDGE('',*,*,#8697,.T.);
#11815=ORIENTED_EDGE('',*,*,#8392,.T.);
#11816=ORIENTED_EDGE('',*,*,#8682,.F.);
#11817=ORIENTED_EDGE('',*,*,#8702,.F.);
#11818=ORIENTED_EDGE('',*,*,#8731,.T.);
#11819=ORIENTED_EDGE('',*,*,#8706,.F.);
#11820=ORIENTED_EDGE('',*,*,#8711,.F.);
#11821=ORIENTED_EDGE('',*,*,#8394,.T.);
#11822=ORIENTED_EDGE('',*,*,#8696,.F.);
#11823=ORIENTED_EDGE('',*,*,#8718,.F.);
#11824=ORIENTED_EDGE('',*,*,#8396,.F.);
#11825=ORIENTED_EDGE('',*,*,#8710,.T.);
#11826=ORIENTED_EDGE('',*,*,#8727,.F.);
#11827=ORIENTED_EDGE('',*,*,#8732,.T.);
#11828=ORIENTED_EDGE('',*,*,#8714,.F.);
#11829=ORIENTED_EDGE('',*,*,#8701,.F.);
#11830=ORIENTED_EDGE('',*,*,#8733,.T.);
#11831=ORIENTED_EDGE('',*,*,#8707,.F.);
#11832=ORIENTED_EDGE('',*,*,#8731,.F.);
#11833=ORIENTED_EDGE('',*,*,#8687,.F.);
#11834=ORIENTED_EDGE('',*,*,#8734,.T.);
#11835=ORIENTED_EDGE('',*,*,#8693,.F.);
#11836=ORIENTED_EDGE('',*,*,#8730,.F.);
#11837=ORIENTED_EDGE('',*,*,#8673,.F.);
#11838=ORIENTED_EDGE('',*,*,#8735,.T.);
#11839=ORIENTED_EDGE('',*,*,#8679,.F.);
#11840=ORIENTED_EDGE('',*,*,#8729,.F.);
#11841=ORIENTED_EDGE('',*,*,#8659,.F.);
#11842=ORIENTED_EDGE('',*,*,#8736,.T.);
#11843=ORIENTED_EDGE('',*,*,#8665,.F.);
#11844=ORIENTED_EDGE('',*,*,#8728,.F.);
#11845=ORIENTED_EDGE('',*,*,#8737,.T.);
#11846=ORIENTED_EDGE('',*,*,#8738,.T.);
#11847=ORIENTED_EDGE('',*,*,#8739,.T.);
#11848=ORIENTED_EDGE('',*,*,#8740,.T.);
#11849=ORIENTED_EDGE('',*,*,#8741,.T.);
#11850=ORIENTED_EDGE('',*,*,#8741,.F.);
#11851=ORIENTED_EDGE('',*,*,#8742,.T.);
#11852=ORIENTED_EDGE('',*,*,#8743,.F.);
#11853=ORIENTED_EDGE('',*,*,#8744,.T.);
#11854=ORIENTED_EDGE('',*,*,#8376,.T.);
#11855=ORIENTED_EDGE('',*,*,#8745,.F.);
#11856=ORIENTED_EDGE('',*,*,#8740,.F.);
#11857=ORIENTED_EDGE('',*,*,#8746,.T.);
#11858=ORIENTED_EDGE('',*,*,#8747,.F.);
#11859=ORIENTED_EDGE('',*,*,#8742,.F.);
#11860=ORIENTED_EDGE('',*,*,#8748,.F.);
#11861=ORIENTED_EDGE('',*,*,#8749,.T.);
#11862=ORIENTED_EDGE('',*,*,#8750,.T.);
#11863=ORIENTED_EDGE('',*,*,#8743,.T.);
#11864=ORIENTED_EDGE('',*,*,#8747,.T.);
#11865=ORIENTED_EDGE('',*,*,#8751,.T.);
#11866=ORIENTED_EDGE('',*,*,#8752,.T.);
#11867=ORIENTED_EDGE('',*,*,#8753,.T.);
#11868=ORIENTED_EDGE('',*,*,#8754,.T.);
#11869=ORIENTED_EDGE('',*,*,#8755,.T.);
#11870=ORIENTED_EDGE('',*,*,#8755,.F.);
#11871=ORIENTED_EDGE('',*,*,#8756,.T.);
#11872=ORIENTED_EDGE('',*,*,#8757,.F.);
#11873=ORIENTED_EDGE('',*,*,#8758,.T.);
#11874=ORIENTED_EDGE('',*,*,#8378,.T.);
#11875=ORIENTED_EDGE('',*,*,#8759,.F.);
#11876=ORIENTED_EDGE('',*,*,#8754,.F.);
#11877=ORIENTED_EDGE('',*,*,#8760,.T.);
#11878=ORIENTED_EDGE('',*,*,#8761,.F.);
#11879=ORIENTED_EDGE('',*,*,#8756,.F.);
#11880=ORIENTED_EDGE('',*,*,#8762,.F.);
#11881=ORIENTED_EDGE('',*,*,#8763,.T.);
#11882=ORIENTED_EDGE('',*,*,#8764,.T.);
#11883=ORIENTED_EDGE('',*,*,#8757,.T.);
#11884=ORIENTED_EDGE('',*,*,#8761,.T.);
#11885=ORIENTED_EDGE('',*,*,#8765,.T.);
#11886=ORIENTED_EDGE('',*,*,#8766,.T.);
#11887=ORIENTED_EDGE('',*,*,#8767,.T.);
#11888=ORIENTED_EDGE('',*,*,#8768,.T.);
#11889=ORIENTED_EDGE('',*,*,#8769,.T.);
#11890=ORIENTED_EDGE('',*,*,#8769,.F.);
#11891=ORIENTED_EDGE('',*,*,#8770,.T.);
#11892=ORIENTED_EDGE('',*,*,#8771,.F.);
#11893=ORIENTED_EDGE('',*,*,#8772,.T.);
#11894=ORIENTED_EDGE('',*,*,#8380,.T.);
#11895=ORIENTED_EDGE('',*,*,#8773,.F.);
#11896=ORIENTED_EDGE('',*,*,#8768,.F.);
#11897=ORIENTED_EDGE('',*,*,#8774,.T.);
#11898=ORIENTED_EDGE('',*,*,#8775,.F.);
#11899=ORIENTED_EDGE('',*,*,#8770,.F.);
#11900=ORIENTED_EDGE('',*,*,#8776,.F.);
#11901=ORIENTED_EDGE('',*,*,#8777,.T.);
#11902=ORIENTED_EDGE('',*,*,#8778,.T.);
#11903=ORIENTED_EDGE('',*,*,#8771,.T.);
#11904=ORIENTED_EDGE('',*,*,#8775,.T.);
#11905=ORIENTED_EDGE('',*,*,#8779,.T.);
#11906=ORIENTED_EDGE('',*,*,#8780,.T.);
#11907=ORIENTED_EDGE('',*,*,#8781,.T.);
#11908=ORIENTED_EDGE('',*,*,#8782,.T.);
#11909=ORIENTED_EDGE('',*,*,#8783,.T.);
#11910=ORIENTED_EDGE('',*,*,#8783,.F.);
#11911=ORIENTED_EDGE('',*,*,#8784,.T.);
#11912=ORIENTED_EDGE('',*,*,#8785,.F.);
#11913=ORIENTED_EDGE('',*,*,#8786,.T.);
#11914=ORIENTED_EDGE('',*,*,#8382,.T.);
#11915=ORIENTED_EDGE('',*,*,#8787,.F.);
#11916=ORIENTED_EDGE('',*,*,#8782,.F.);
#11917=ORIENTED_EDGE('',*,*,#8788,.T.);
#11918=ORIENTED_EDGE('',*,*,#8789,.F.);
#11919=ORIENTED_EDGE('',*,*,#8784,.F.);
#11920=ORIENTED_EDGE('',*,*,#8790,.F.);
#11921=ORIENTED_EDGE('',*,*,#8791,.T.);
#11922=ORIENTED_EDGE('',*,*,#8792,.T.);
#11923=ORIENTED_EDGE('',*,*,#8785,.T.);
#11924=ORIENTED_EDGE('',*,*,#8789,.T.);
#11925=ORIENTED_EDGE('',*,*,#8793,.T.);
#11926=ORIENTED_EDGE('',*,*,#8794,.T.);
#11927=ORIENTED_EDGE('',*,*,#8795,.T.);
#11928=ORIENTED_EDGE('',*,*,#8796,.T.);
#11929=ORIENTED_EDGE('',*,*,#8797,.T.);
#11930=ORIENTED_EDGE('',*,*,#8797,.F.);
#11931=ORIENTED_EDGE('',*,*,#8798,.T.);
#11932=ORIENTED_EDGE('',*,*,#8799,.F.);
#11933=ORIENTED_EDGE('',*,*,#8800,.T.);
#11934=ORIENTED_EDGE('',*,*,#8384,.T.);
#11935=ORIENTED_EDGE('',*,*,#8801,.F.);
#11936=ORIENTED_EDGE('',*,*,#8796,.F.);
#11937=ORIENTED_EDGE('',*,*,#8802,.T.);
#11938=ORIENTED_EDGE('',*,*,#8803,.F.);
#11939=ORIENTED_EDGE('',*,*,#8798,.F.);
#11940=ORIENTED_EDGE('',*,*,#8804,.T.);
#11941=ORIENTED_EDGE('',*,*,#8805,.T.);
#11942=ORIENTED_EDGE('',*,*,#8806,.T.);
#11943=ORIENTED_EDGE('',*,*,#8807,.T.);
#11944=ORIENTED_EDGE('',*,*,#8805,.F.);
#11945=ORIENTED_EDGE('',*,*,#8808,.F.);
#11946=ORIENTED_EDGE('',*,*,#8809,.F.);
#11947=ORIENTED_EDGE('',*,*,#8810,.F.);
#11948=ORIENTED_EDGE('',*,*,#8804,.F.);
#11949=ORIENTED_EDGE('',*,*,#8811,.F.);
#11950=ORIENTED_EDGE('',*,*,#8385,.T.);
#11951=ORIENTED_EDGE('',*,*,#8800,.F.);
#11952=ORIENTED_EDGE('',*,*,#8812,.F.);
#11953=ORIENTED_EDGE('',*,*,#8808,.T.);
#11954=ORIENTED_EDGE('',*,*,#8813,.F.);
#11955=ORIENTED_EDGE('',*,*,#8809,.T.);
#11956=ORIENTED_EDGE('',*,*,#8812,.T.);
#11957=ORIENTED_EDGE('',*,*,#8799,.T.);
#11958=ORIENTED_EDGE('',*,*,#8803,.T.);
#11959=ORIENTED_EDGE('',*,*,#8814,.F.);
#11960=ORIENTED_EDGE('',*,*,#8815,.T.);
#11961=ORIENTED_EDGE('',*,*,#8816,.T.);
#11962=ORIENTED_EDGE('',*,*,#8817,.T.);
#11963=ORIENTED_EDGE('',*,*,#8816,.F.);
#11964=ORIENTED_EDGE('',*,*,#8818,.T.);
#11965=ORIENTED_EDGE('',*,*,#8819,.F.);
#11966=ORIENTED_EDGE('',*,*,#8820,.T.);
#11967=ORIENTED_EDGE('',*,*,#8367,.T.);
#11968=ORIENTED_EDGE('',*,*,#8821,.F.);
#11969=ORIENTED_EDGE('',*,*,#8815,.F.);
#11970=ORIENTED_EDGE('',*,*,#8822,.F.);
#11971=ORIENTED_EDGE('',*,*,#8823,.F.);
#11972=ORIENTED_EDGE('',*,*,#8818,.F.);
#11973=ORIENTED_EDGE('',*,*,#8819,.T.);
#11974=ORIENTED_EDGE('',*,*,#8823,.T.);
#11975=ORIENTED_EDGE('',*,*,#8824,.T.);
#11976=ORIENTED_EDGE('',*,*,#8825,.T.);
#11977=ORIENTED_EDGE('',*,*,#8826,.T.);
#11978=ORIENTED_EDGE('',*,*,#8827,.F.);
#11979=ORIENTED_EDGE('',*,*,#8828,.T.);
#11980=ORIENTED_EDGE('',*,*,#8829,.T.);
#11981=ORIENTED_EDGE('',*,*,#8830,.T.);
#11982=ORIENTED_EDGE('',*,*,#8831,.T.);
#11983=ORIENTED_EDGE('',*,*,#8829,.F.);
#11984=ORIENTED_EDGE('',*,*,#8832,.T.);
#11985=ORIENTED_EDGE('',*,*,#8833,.F.);
#11986=ORIENTED_EDGE('',*,*,#8834,.T.);
#11987=ORIENTED_EDGE('',*,*,#8369,.T.);
#11988=ORIENTED_EDGE('',*,*,#8835,.F.);
#11989=ORIENTED_EDGE('',*,*,#8828,.F.);
#11990=ORIENTED_EDGE('',*,*,#8836,.F.);
#11991=ORIENTED_EDGE('',*,*,#8837,.F.);
#11992=ORIENTED_EDGE('',*,*,#8832,.F.);
#11993=ORIENTED_EDGE('',*,*,#8833,.T.);
#11994=ORIENTED_EDGE('',*,*,#8837,.T.);
#11995=ORIENTED_EDGE('',*,*,#8838,.T.);
#11996=ORIENTED_EDGE('',*,*,#8839,.T.);
#11997=ORIENTED_EDGE('',*,*,#8840,.T.);
#11998=ORIENTED_EDGE('',*,*,#8841,.F.);
#11999=ORIENTED_EDGE('',*,*,#8842,.T.);
#12000=ORIENTED_EDGE('',*,*,#8843,.T.);
#12001=ORIENTED_EDGE('',*,*,#8844,.T.);
#12002=ORIENTED_EDGE('',*,*,#8845,.T.);
#12003=ORIENTED_EDGE('',*,*,#8843,.F.);
#12004=ORIENTED_EDGE('',*,*,#8846,.T.);
#12005=ORIENTED_EDGE('',*,*,#8847,.F.);
#12006=ORIENTED_EDGE('',*,*,#8848,.T.);
#12007=ORIENTED_EDGE('',*,*,#8371,.T.);
#12008=ORIENTED_EDGE('',*,*,#8849,.F.);
#12009=ORIENTED_EDGE('',*,*,#8842,.F.);
#12010=ORIENTED_EDGE('',*,*,#8850,.F.);
#12011=ORIENTED_EDGE('',*,*,#8851,.F.);
#12012=ORIENTED_EDGE('',*,*,#8846,.F.);
#12013=ORIENTED_EDGE('',*,*,#8847,.T.);
#12014=ORIENTED_EDGE('',*,*,#8851,.T.);
#12015=ORIENTED_EDGE('',*,*,#8852,.T.);
#12016=ORIENTED_EDGE('',*,*,#8853,.T.);
#12017=ORIENTED_EDGE('',*,*,#8854,.T.);
#12018=ORIENTED_EDGE('',*,*,#8855,.F.);
#12019=ORIENTED_EDGE('',*,*,#8856,.T.);
#12020=ORIENTED_EDGE('',*,*,#8857,.T.);
#12021=ORIENTED_EDGE('',*,*,#8858,.T.);
#12022=ORIENTED_EDGE('',*,*,#8859,.T.);
#12023=ORIENTED_EDGE('',*,*,#8857,.F.);
#12024=ORIENTED_EDGE('',*,*,#8860,.T.);
#12025=ORIENTED_EDGE('',*,*,#8861,.F.);
#12026=ORIENTED_EDGE('',*,*,#8862,.F.);
#12027=ORIENTED_EDGE('',*,*,#8373,.T.);
#12028=ORIENTED_EDGE('',*,*,#8863,.F.);
#12029=ORIENTED_EDGE('',*,*,#8856,.F.);
#12030=ORIENTED_EDGE('',*,*,#8864,.F.);
#12031=ORIENTED_EDGE('',*,*,#8865,.F.);
#12032=ORIENTED_EDGE('',*,*,#8860,.F.);
#12033=ORIENTED_EDGE('',*,*,#8866,.T.);
#12034=ORIENTED_EDGE('',*,*,#8867,.F.);
#12035=ORIENTED_EDGE('',*,*,#8868,.T.);
#12036=ORIENTED_EDGE('',*,*,#8869,.T.);
#12037=ORIENTED_EDGE('',*,*,#8737,.F.);
#12038=ORIENTED_EDGE('',*,*,#8745,.T.);
#12039=ORIENTED_EDGE('',*,*,#8375,.T.);
#12040=ORIENTED_EDGE('',*,*,#8870,.T.);
#12041=ORIENTED_EDGE('',*,*,#8869,.F.);
#12042=ORIENTED_EDGE('',*,*,#8871,.T.);
#12043=ORIENTED_EDGE('',*,*,#8750,.F.);
#12044=ORIENTED_EDGE('',*,*,#8872,.T.);
#12045=ORIENTED_EDGE('',*,*,#8751,.F.);
#12046=ORIENTED_EDGE('',*,*,#8759,.T.);
#12047=ORIENTED_EDGE('',*,*,#8377,.T.);
#12048=ORIENTED_EDGE('',*,*,#8744,.F.);
#12049=ORIENTED_EDGE('',*,*,#8764,.F.);
#12050=ORIENTED_EDGE('',*,*,#8873,.T.);
#12051=ORIENTED_EDGE('',*,*,#8765,.F.);
#12052=ORIENTED_EDGE('',*,*,#8773,.T.);
#12053=ORIENTED_EDGE('',*,*,#8379,.T.);
#12054=ORIENTED_EDGE('',*,*,#8758,.F.);
#12055=ORIENTED_EDGE('',*,*,#8778,.F.);
#12056=ORIENTED_EDGE('',*,*,#8874,.T.);
#12057=ORIENTED_EDGE('',*,*,#8779,.F.);
#12058=ORIENTED_EDGE('',*,*,#8787,.T.);
#12059=ORIENTED_EDGE('',*,*,#8381,.T.);
#12060=ORIENTED_EDGE('',*,*,#8772,.F.);
#12061=ORIENTED_EDGE('',*,*,#8792,.F.);
#12062=ORIENTED_EDGE('',*,*,#8875,.T.);
#12063=ORIENTED_EDGE('',*,*,#8793,.F.);
#12064=ORIENTED_EDGE('',*,*,#8801,.T.);
#12065=ORIENTED_EDGE('',*,*,#8383,.T.);
#12066=ORIENTED_EDGE('',*,*,#8786,.F.);
#12067=ORIENTED_EDGE('',*,*,#8791,.F.);
#12068=ORIENTED_EDGE('',*,*,#8876,.F.);
#12069=ORIENTED_EDGE('',*,*,#8794,.F.);
#12070=ORIENTED_EDGE('',*,*,#8875,.F.);
#12071=ORIENTED_EDGE('',*,*,#8777,.F.);
#12072=ORIENTED_EDGE('',*,*,#8877,.F.);
#12073=ORIENTED_EDGE('',*,*,#8780,.F.);
#12074=ORIENTED_EDGE('',*,*,#8874,.F.);
#12075=ORIENTED_EDGE('',*,*,#8763,.F.);
#12076=ORIENTED_EDGE('',*,*,#8878,.F.);
#12077=ORIENTED_EDGE('',*,*,#8766,.F.);
#12078=ORIENTED_EDGE('',*,*,#8873,.F.);
#12079=ORIENTED_EDGE('',*,*,#8749,.F.);
#12080=ORIENTED_EDGE('',*,*,#8879,.F.);
#12081=ORIENTED_EDGE('',*,*,#8752,.F.);
#12082=ORIENTED_EDGE('',*,*,#8872,.F.);
#12083=ORIENTED_EDGE('',*,*,#8738,.F.);
#12084=ORIENTED_EDGE('',*,*,#8871,.F.);
#12085=ORIENTED_EDGE('',*,*,#8868,.F.);
#12086=ORIENTED_EDGE('',*,*,#8880,.F.);
#12087=ORIENTED_EDGE('',*,*,#8861,.T.);
#12088=ORIENTED_EDGE('',*,*,#8865,.T.);
#12089=ORIENTED_EDGE('',*,*,#8881,.T.);
#12090=ORIENTED_EDGE('',*,*,#8882,.T.);
#12091=ORIENTED_EDGE('',*,*,#8826,.F.);
#12092=ORIENTED_EDGE('',*,*,#8883,.T.);
#12093=ORIENTED_EDGE('',*,*,#8830,.F.);
#12094=ORIENTED_EDGE('',*,*,#8835,.T.);
#12095=ORIENTED_EDGE('',*,*,#8368,.T.);
#12096=ORIENTED_EDGE('',*,*,#8820,.F.);
#12097=ORIENTED_EDGE('',*,*,#8840,.F.);
#12098=ORIENTED_EDGE('',*,*,#8884,.T.);
#12099=ORIENTED_EDGE('',*,*,#8844,.F.);
#12100=ORIENTED_EDGE('',*,*,#8849,.T.);
#12101=ORIENTED_EDGE('',*,*,#8370,.T.);
#12102=ORIENTED_EDGE('',*,*,#8834,.F.);
#12103=ORIENTED_EDGE('',*,*,#8854,.F.);
#12104=ORIENTED_EDGE('',*,*,#8885,.T.);
#12105=ORIENTED_EDGE('',*,*,#8858,.F.);
#12106=ORIENTED_EDGE('',*,*,#8863,.T.);
#12107=ORIENTED_EDGE('',*,*,#8372,.T.);
#12108=ORIENTED_EDGE('',*,*,#8848,.F.);
#12109=ORIENTED_EDGE('',*,*,#8870,.F.);
#12110=ORIENTED_EDGE('',*,*,#8374,.F.);
#12111=ORIENTED_EDGE('',*,*,#8862,.T.);
#12112=ORIENTED_EDGE('',*,*,#8882,.F.);
#12113=ORIENTED_EDGE('',*,*,#8886,.T.);
#12114=ORIENTED_EDGE('',*,*,#8866,.F.);
#12115=ORIENTED_EDGE('',*,*,#8853,.F.);
#12116=ORIENTED_EDGE('',*,*,#8887,.T.);
#12117=ORIENTED_EDGE('',*,*,#8859,.F.);
#12118=ORIENTED_EDGE('',*,*,#8885,.F.);
#12119=ORIENTED_EDGE('',*,*,#8839,.F.);
#12120=ORIENTED_EDGE('',*,*,#8888,.T.);
#12121=ORIENTED_EDGE('',*,*,#8845,.F.);
#12122=ORIENTED_EDGE('',*,*,#8884,.F.);
#12123=ORIENTED_EDGE('',*,*,#8825,.F.);
#12124=ORIENTED_EDGE('',*,*,#8889,.T.);
#12125=ORIENTED_EDGE('',*,*,#8831,.F.);
#12126=ORIENTED_EDGE('',*,*,#8883,.F.);
#12127=ORIENTED_EDGE('',*,*,#8890,.T.);
#12128=ORIENTED_EDGE('',*,*,#8891,.T.);
#12129=ORIENTED_EDGE('',*,*,#8892,.T.);
#12130=ORIENTED_EDGE('',*,*,#8893,.T.);
#12131=ORIENTED_EDGE('',*,*,#8894,.T.);
#12132=ORIENTED_EDGE('',*,*,#8894,.F.);
#12133=ORIENTED_EDGE('',*,*,#8895,.T.);
#12134=ORIENTED_EDGE('',*,*,#8896,.F.);
#12135=ORIENTED_EDGE('',*,*,#8897,.F.);
#12136=ORIENTED_EDGE('',*,*,#8354,.T.);
#12137=ORIENTED_EDGE('',*,*,#8898,.F.);
#12138=ORIENTED_EDGE('',*,*,#8893,.F.);
#12139=ORIENTED_EDGE('',*,*,#8899,.T.);
#12140=ORIENTED_EDGE('',*,*,#8900,.F.);
#12141=ORIENTED_EDGE('',*,*,#8895,.F.);
#12142=ORIENTED_EDGE('',*,*,#8901,.F.);
#12143=ORIENTED_EDGE('',*,*,#8902,.T.);
#12144=ORIENTED_EDGE('',*,*,#8903,.T.);
#12145=ORIENTED_EDGE('',*,*,#8896,.T.);
#12146=ORIENTED_EDGE('',*,*,#8900,.T.);
#12147=ORIENTED_EDGE('',*,*,#8903,.F.);
#12148=ORIENTED_EDGE('',*,*,#8904,.T.);
#12149=ORIENTED_EDGE('',*,*,#8905,.F.);
#12150=ORIENTED_EDGE('',*,*,#8906,.T.);
#12151=ORIENTED_EDGE('',*,*,#8355,.T.);
#12152=ORIENTED_EDGE('',*,*,#8897,.T.);
#12153=ORIENTED_EDGE('',*,*,#8905,.T.);
#12154=ORIENTED_EDGE('',*,*,#8907,.T.);
#12155=ORIENTED_EDGE('',*,*,#8908,.T.);
#12156=ORIENTED_EDGE('',*,*,#8909,.T.);
#12157=ORIENTED_EDGE('',*,*,#8910,.T.);
#12158=ORIENTED_EDGE('',*,*,#8910,.F.);
#12159=ORIENTED_EDGE('',*,*,#8911,.T.);
#12160=ORIENTED_EDGE('',*,*,#8912,.F.);
#12161=ORIENTED_EDGE('',*,*,#8913,.T.);
#12162=ORIENTED_EDGE('',*,*,#8356,.T.);
#12163=ORIENTED_EDGE('',*,*,#8906,.F.);
#12164=ORIENTED_EDGE('',*,*,#8909,.F.);
#12165=ORIENTED_EDGE('',*,*,#8914,.T.);
#12166=ORIENTED_EDGE('',*,*,#8915,.F.);
#12167=ORIENTED_EDGE('',*,*,#8911,.F.);
#12168=ORIENTED_EDGE('',*,*,#8916,.F.);
#12169=ORIENTED_EDGE('',*,*,#8917,.T.);
#12170=ORIENTED_EDGE('',*,*,#8918,.T.);
#12171=ORIENTED_EDGE('',*,*,#8912,.T.);
#12172=ORIENTED_EDGE('',*,*,#8915,.T.);
#12173=ORIENTED_EDGE('',*,*,#8919,.T.);
#12174=ORIENTED_EDGE('',*,*,#8920,.T.);
#12175=ORIENTED_EDGE('',*,*,#8921,.T.);
#12176=ORIENTED_EDGE('',*,*,#8922,.T.);
#12177=ORIENTED_EDGE('',*,*,#8923,.T.);
#12178=ORIENTED_EDGE('',*,*,#8923,.F.);
#12179=ORIENTED_EDGE('',*,*,#8924,.T.);
#12180=ORIENTED_EDGE('',*,*,#8925,.F.);
#12181=ORIENTED_EDGE('',*,*,#8926,.T.);
#12182=ORIENTED_EDGE('',*,*,#8358,.T.);
#12183=ORIENTED_EDGE('',*,*,#8927,.F.);
#12184=ORIENTED_EDGE('',*,*,#8922,.F.);
#12185=ORIENTED_EDGE('',*,*,#8928,.T.);
#12186=ORIENTED_EDGE('',*,*,#8929,.F.);
#12187=ORIENTED_EDGE('',*,*,#8924,.F.);
#12188=ORIENTED_EDGE('',*,*,#8930,.F.);
#12189=ORIENTED_EDGE('',*,*,#8931,.T.);
#12190=ORIENTED_EDGE('',*,*,#8932,.T.);
#12191=ORIENTED_EDGE('',*,*,#8925,.T.);
#12192=ORIENTED_EDGE('',*,*,#8929,.T.);
#12193=ORIENTED_EDGE('',*,*,#8933,.T.);
#12194=ORIENTED_EDGE('',*,*,#8934,.T.);
#12195=ORIENTED_EDGE('',*,*,#8935,.T.);
#12196=ORIENTED_EDGE('',*,*,#8936,.T.);
#12197=ORIENTED_EDGE('',*,*,#8937,.T.);
#12198=ORIENTED_EDGE('',*,*,#8937,.F.);
#12199=ORIENTED_EDGE('',*,*,#8938,.T.);
#12200=ORIENTED_EDGE('',*,*,#8939,.F.);
#12201=ORIENTED_EDGE('',*,*,#8940,.T.);
#12202=ORIENTED_EDGE('',*,*,#8360,.T.);
#12203=ORIENTED_EDGE('',*,*,#8941,.F.);
#12204=ORIENTED_EDGE('',*,*,#8936,.F.);
#12205=ORIENTED_EDGE('',*,*,#8942,.T.);
#12206=ORIENTED_EDGE('',*,*,#8943,.F.);
#12207=ORIENTED_EDGE('',*,*,#8938,.F.);
#12208=ORIENTED_EDGE('',*,*,#8944,.F.);
#12209=ORIENTED_EDGE('',*,*,#8945,.T.);
#12210=ORIENTED_EDGE('',*,*,#8946,.T.);
#12211=ORIENTED_EDGE('',*,*,#8939,.T.);
#12212=ORIENTED_EDGE('',*,*,#8943,.T.);
#12213=ORIENTED_EDGE('',*,*,#8947,.T.);
#12214=ORIENTED_EDGE('',*,*,#8948,.T.);
#12215=ORIENTED_EDGE('',*,*,#8949,.T.);
#12216=ORIENTED_EDGE('',*,*,#8950,.T.);
#12217=ORIENTED_EDGE('',*,*,#8951,.T.);
#12218=ORIENTED_EDGE('',*,*,#8951,.F.);
#12219=ORIENTED_EDGE('',*,*,#8952,.T.);
#12220=ORIENTED_EDGE('',*,*,#8953,.F.);
#12221=ORIENTED_EDGE('',*,*,#8954,.T.);
#12222=ORIENTED_EDGE('',*,*,#8362,.T.);
#12223=ORIENTED_EDGE('',*,*,#8955,.F.);
#12224=ORIENTED_EDGE('',*,*,#8950,.F.);
#12225=ORIENTED_EDGE('',*,*,#8956,.T.);
#12226=ORIENTED_EDGE('',*,*,#8957,.F.);
#12227=ORIENTED_EDGE('',*,*,#8952,.F.);
#12228=ORIENTED_EDGE('',*,*,#8958,.F.);
#12229=ORIENTED_EDGE('',*,*,#8959,.T.);
#12230=ORIENTED_EDGE('',*,*,#8960,.T.);
#12231=ORIENTED_EDGE('',*,*,#8953,.T.);
#12232=ORIENTED_EDGE('',*,*,#8957,.T.);
#12233=ORIENTED_EDGE('',*,*,#8961,.T.);
#12234=ORIENTED_EDGE('',*,*,#8962,.T.);
#12235=ORIENTED_EDGE('',*,*,#8963,.T.);
#12236=ORIENTED_EDGE('',*,*,#8964,.T.);
#12237=ORIENTED_EDGE('',*,*,#8965,.T.);
#12238=ORIENTED_EDGE('',*,*,#8965,.F.);
#12239=ORIENTED_EDGE('',*,*,#8966,.T.);
#12240=ORIENTED_EDGE('',*,*,#8967,.F.);
#12241=ORIENTED_EDGE('',*,*,#8968,.T.);
#12242=ORIENTED_EDGE('',*,*,#8364,.T.);
#12243=ORIENTED_EDGE('',*,*,#8969,.F.);
#12244=ORIENTED_EDGE('',*,*,#8964,.F.);
#12245=ORIENTED_EDGE('',*,*,#8970,.T.);
#12246=ORIENTED_EDGE('',*,*,#8971,.F.);
#12247=ORIENTED_EDGE('',*,*,#8966,.F.);
#12248=ORIENTED_EDGE('',*,*,#8972,.T.);
#12249=ORIENTED_EDGE('',*,*,#8973,.T.);
#12250=ORIENTED_EDGE('',*,*,#8974,.T.);
#12251=ORIENTED_EDGE('',*,*,#8975,.T.);
#12252=ORIENTED_EDGE('',*,*,#8973,.F.);
#12253=ORIENTED_EDGE('',*,*,#8976,.F.);
#12254=ORIENTED_EDGE('',*,*,#8977,.F.);
#12255=ORIENTED_EDGE('',*,*,#8978,.F.);
#12256=ORIENTED_EDGE('',*,*,#8972,.F.);
#12257=ORIENTED_EDGE('',*,*,#8979,.F.);
#12258=ORIENTED_EDGE('',*,*,#8365,.T.);
#12259=ORIENTED_EDGE('',*,*,#8968,.F.);
#12260=ORIENTED_EDGE('',*,*,#8980,.F.);
#12261=ORIENTED_EDGE('',*,*,#8976,.T.);
#12262=ORIENTED_EDGE('',*,*,#8981,.F.);
#12263=ORIENTED_EDGE('',*,*,#8977,.T.);
#12264=ORIENTED_EDGE('',*,*,#8980,.T.);
#12265=ORIENTED_EDGE('',*,*,#8967,.T.);
#12266=ORIENTED_EDGE('',*,*,#8971,.T.);
#12267=ORIENTED_EDGE('',*,*,#8982,.F.);
#12268=ORIENTED_EDGE('',*,*,#8983,.T.);
#12269=ORIENTED_EDGE('',*,*,#8984,.T.);
#12270=ORIENTED_EDGE('',*,*,#8985,.T.);
#12271=ORIENTED_EDGE('',*,*,#8984,.F.);
#12272=ORIENTED_EDGE('',*,*,#8986,.T.);
#12273=ORIENTED_EDGE('',*,*,#8987,.F.);
#12274=ORIENTED_EDGE('',*,*,#8988,.T.);
#12275=ORIENTED_EDGE('',*,*,#8347,.T.);
#12276=ORIENTED_EDGE('',*,*,#8989,.F.);
#12277=ORIENTED_EDGE('',*,*,#8983,.F.);
#12278=ORIENTED_EDGE('',*,*,#8990,.F.);
#12279=ORIENTED_EDGE('',*,*,#8991,.F.);
#12280=ORIENTED_EDGE('',*,*,#8986,.F.);
#12281=ORIENTED_EDGE('',*,*,#8987,.T.);
#12282=ORIENTED_EDGE('',*,*,#8991,.T.);
#12283=ORIENTED_EDGE('',*,*,#8992,.T.);
#12284=ORIENTED_EDGE('',*,*,#8993,.T.);
#12285=ORIENTED_EDGE('',*,*,#8994,.T.);
#12286=ORIENTED_EDGE('',*,*,#8995,.F.);
#12287=ORIENTED_EDGE('',*,*,#8996,.T.);
#12288=ORIENTED_EDGE('',*,*,#8997,.T.);
#12289=ORIENTED_EDGE('',*,*,#8998,.T.);
#12290=ORIENTED_EDGE('',*,*,#8999,.T.);
#12291=ORIENTED_EDGE('',*,*,#8997,.F.);
#12292=ORIENTED_EDGE('',*,*,#9000,.T.);
#12293=ORIENTED_EDGE('',*,*,#9001,.F.);
#12294=ORIENTED_EDGE('',*,*,#9002,.T.);
#12295=ORIENTED_EDGE('',*,*,#8349,.T.);
#12296=ORIENTED_EDGE('',*,*,#9003,.F.);
#12297=ORIENTED_EDGE('',*,*,#8996,.F.);
#12298=ORIENTED_EDGE('',*,*,#9004,.F.);
#12299=ORIENTED_EDGE('',*,*,#9005,.F.);
#12300=ORIENTED_EDGE('',*,*,#9000,.F.);
#12301=ORIENTED_EDGE('',*,*,#9001,.T.);
#12302=ORIENTED_EDGE('',*,*,#9005,.T.);
#12303=ORIENTED_EDGE('',*,*,#9006,.T.);
#12304=ORIENTED_EDGE('',*,*,#9007,.T.);
#12305=ORIENTED_EDGE('',*,*,#9008,.T.);
#12306=ORIENTED_EDGE('',*,*,#9009,.F.);
#12307=ORIENTED_EDGE('',*,*,#9010,.T.);
#12308=ORIENTED_EDGE('',*,*,#9011,.T.);
#12309=ORIENTED_EDGE('',*,*,#9012,.T.);
#12310=ORIENTED_EDGE('',*,*,#9013,.T.);
#12311=ORIENTED_EDGE('',*,*,#9011,.F.);
#12312=ORIENTED_EDGE('',*,*,#9014,.T.);
#12313=ORIENTED_EDGE('',*,*,#9015,.F.);
#12314=ORIENTED_EDGE('',*,*,#9016,.F.);
#12315=ORIENTED_EDGE('',*,*,#8351,.T.);
#12316=ORIENTED_EDGE('',*,*,#9017,.T.);
#12317=ORIENTED_EDGE('',*,*,#9010,.F.);
#12318=ORIENTED_EDGE('',*,*,#9018,.F.);
#12319=ORIENTED_EDGE('',*,*,#9019,.F.);
#12320=ORIENTED_EDGE('',*,*,#9014,.F.);
#12321=ORIENTED_EDGE('',*,*,#9020,.T.);
#12322=ORIENTED_EDGE('',*,*,#9021,.F.);
#12323=ORIENTED_EDGE('',*,*,#9022,.T.);
#12324=ORIENTED_EDGE('',*,*,#9023,.T.);
#12325=ORIENTED_EDGE('',*,*,#8890,.F.);
#12326=ORIENTED_EDGE('',*,*,#8898,.T.);
#12327=ORIENTED_EDGE('',*,*,#8353,.T.);
#12328=ORIENTED_EDGE('',*,*,#9024,.T.);
#12329=ORIENTED_EDGE('',*,*,#9023,.F.);
#12330=ORIENTED_EDGE('',*,*,#9025,.T.);
#12331=ORIENTED_EDGE('',*,*,#8918,.F.);
#12332=ORIENTED_EDGE('',*,*,#9026,.T.);
#12333=ORIENTED_EDGE('',*,*,#8919,.F.);
#12334=ORIENTED_EDGE('',*,*,#8927,.T.);
#12335=ORIENTED_EDGE('',*,*,#8357,.T.);
#12336=ORIENTED_EDGE('',*,*,#8913,.F.);
#12337=ORIENTED_EDGE('',*,*,#8932,.F.);
#12338=ORIENTED_EDGE('',*,*,#9027,.T.);
#12339=ORIENTED_EDGE('',*,*,#8933,.F.);
#12340=ORIENTED_EDGE('',*,*,#8941,.T.);
#12341=ORIENTED_EDGE('',*,*,#8359,.T.);
#12342=ORIENTED_EDGE('',*,*,#8926,.F.);
#12343=ORIENTED_EDGE('',*,*,#8946,.F.);
#12344=ORIENTED_EDGE('',*,*,#9028,.T.);
#12345=ORIENTED_EDGE('',*,*,#8947,.F.);
#12346=ORIENTED_EDGE('',*,*,#8955,.T.);
#12347=ORIENTED_EDGE('',*,*,#8361,.T.);
#12348=ORIENTED_EDGE('',*,*,#8940,.F.);
#12349=ORIENTED_EDGE('',*,*,#8960,.F.);
#12350=ORIENTED_EDGE('',*,*,#9029,.T.);
#12351=ORIENTED_EDGE('',*,*,#8961,.F.);
#12352=ORIENTED_EDGE('',*,*,#8969,.T.);
#12353=ORIENTED_EDGE('',*,*,#8363,.T.);
#12354=ORIENTED_EDGE('',*,*,#8954,.F.);
#12355=ORIENTED_EDGE('',*,*,#8959,.F.);
#12356=ORIENTED_EDGE('',*,*,#9030,.F.);
#12357=ORIENTED_EDGE('',*,*,#8962,.F.);
#12358=ORIENTED_EDGE('',*,*,#9029,.F.);
#12359=ORIENTED_EDGE('',*,*,#8945,.F.);
#12360=ORIENTED_EDGE('',*,*,#9031,.F.);
#12361=ORIENTED_EDGE('',*,*,#8948,.F.);
#12362=ORIENTED_EDGE('',*,*,#9028,.F.);
#12363=ORIENTED_EDGE('',*,*,#8931,.F.);
#12364=ORIENTED_EDGE('',*,*,#9032,.F.);
#12365=ORIENTED_EDGE('',*,*,#8934,.F.);
#12366=ORIENTED_EDGE('',*,*,#9027,.F.);
#12367=ORIENTED_EDGE('',*,*,#8917,.F.);
#12368=ORIENTED_EDGE('',*,*,#9033,.F.);
#12369=ORIENTED_EDGE('',*,*,#8920,.F.);
#12370=ORIENTED_EDGE('',*,*,#9026,.F.);
#12371=ORIENTED_EDGE('',*,*,#8902,.F.);
#12372=ORIENTED_EDGE('',*,*,#9034,.F.);
#12373=ORIENTED_EDGE('',*,*,#8907,.F.);
#12374=ORIENTED_EDGE('',*,*,#8904,.F.);
#12375=ORIENTED_EDGE('',*,*,#8891,.F.);
#12376=ORIENTED_EDGE('',*,*,#9025,.F.);
#12377=ORIENTED_EDGE('',*,*,#9022,.F.);
#12378=ORIENTED_EDGE('',*,*,#9035,.F.);
#12379=ORIENTED_EDGE('',*,*,#9015,.T.);
#12380=ORIENTED_EDGE('',*,*,#9019,.T.);
#12381=ORIENTED_EDGE('',*,*,#9036,.T.);
#12382=ORIENTED_EDGE('',*,*,#9037,.T.);
#12383=ORIENTED_EDGE('',*,*,#8994,.F.);
#12384=ORIENTED_EDGE('',*,*,#9038,.T.);
#12385=ORIENTED_EDGE('',*,*,#8998,.F.);
#12386=ORIENTED_EDGE('',*,*,#9003,.T.);
#12387=ORIENTED_EDGE('',*,*,#8348,.T.);
#12388=ORIENTED_EDGE('',*,*,#8988,.F.);
#12389=ORIENTED_EDGE('',*,*,#9008,.F.);
#12390=ORIENTED_EDGE('',*,*,#9039,.T.);
#12391=ORIENTED_EDGE('',*,*,#9012,.F.);
#12392=ORIENTED_EDGE('',*,*,#9017,.F.);
#12393=ORIENTED_EDGE('',*,*,#8350,.T.);
#12394=ORIENTED_EDGE('',*,*,#9002,.F.);
#12395=ORIENTED_EDGE('',*,*,#9024,.F.);
#12396=ORIENTED_EDGE('',*,*,#8352,.F.);
#12397=ORIENTED_EDGE('',*,*,#9016,.T.);
#12398=ORIENTED_EDGE('',*,*,#9037,.F.);
#12399=ORIENTED_EDGE('',*,*,#9040,.T.);
#12400=ORIENTED_EDGE('',*,*,#9020,.F.);
#12401=ORIENTED_EDGE('',*,*,#9007,.F.);
#12402=ORIENTED_EDGE('',*,*,#9041,.T.);
#12403=ORIENTED_EDGE('',*,*,#9013,.F.);
#12404=ORIENTED_EDGE('',*,*,#9039,.F.);
#12405=ORIENTED_EDGE('',*,*,#8993,.F.);
#12406=ORIENTED_EDGE('',*,*,#9042,.T.);
#12407=ORIENTED_EDGE('',*,*,#8999,.F.);
#12408=ORIENTED_EDGE('',*,*,#9038,.F.);
#12409=ORIENTED_EDGE('',*,*,#9043,.T.);
#12410=ORIENTED_EDGE('',*,*,#9044,.T.);
#12411=ORIENTED_EDGE('',*,*,#9045,.T.);
#12412=ORIENTED_EDGE('',*,*,#9046,.T.);
#12413=ORIENTED_EDGE('',*,*,#9047,.T.);
#12414=ORIENTED_EDGE('',*,*,#9047,.F.);
#12415=ORIENTED_EDGE('',*,*,#9048,.T.);
#12416=ORIENTED_EDGE('',*,*,#9049,.F.);
#12417=ORIENTED_EDGE('',*,*,#9050,.T.);
#12418=ORIENTED_EDGE('',*,*,#8332,.T.);
#12419=ORIENTED_EDGE('',*,*,#9051,.F.);
#12420=ORIENTED_EDGE('',*,*,#9046,.F.);
#12421=ORIENTED_EDGE('',*,*,#9052,.T.);
#12422=ORIENTED_EDGE('',*,*,#9053,.F.);
#12423=ORIENTED_EDGE('',*,*,#9048,.F.);
#12424=ORIENTED_EDGE('',*,*,#9054,.F.);
#12425=ORIENTED_EDGE('',*,*,#9055,.T.);
#12426=ORIENTED_EDGE('',*,*,#9056,.T.);
#12427=ORIENTED_EDGE('',*,*,#9049,.T.);
#12428=ORIENTED_EDGE('',*,*,#9053,.T.);
#12429=ORIENTED_EDGE('',*,*,#9057,.T.);
#12430=ORIENTED_EDGE('',*,*,#9058,.T.);
#12431=ORIENTED_EDGE('',*,*,#9059,.T.);
#12432=ORIENTED_EDGE('',*,*,#9060,.T.);
#12433=ORIENTED_EDGE('',*,*,#9061,.T.);
#12434=ORIENTED_EDGE('',*,*,#9061,.F.);
#12435=ORIENTED_EDGE('',*,*,#9062,.T.);
#12436=ORIENTED_EDGE('',*,*,#9063,.F.);
#12437=ORIENTED_EDGE('',*,*,#9064,.T.);
#12438=ORIENTED_EDGE('',*,*,#8334,.T.);
#12439=ORIENTED_EDGE('',*,*,#9065,.F.);
#12440=ORIENTED_EDGE('',*,*,#9060,.F.);
#12441=ORIENTED_EDGE('',*,*,#9066,.T.);
#12442=ORIENTED_EDGE('',*,*,#9067,.F.);
#12443=ORIENTED_EDGE('',*,*,#9062,.F.);
#12444=ORIENTED_EDGE('',*,*,#9068,.F.);
#12445=ORIENTED_EDGE('',*,*,#9069,.T.);
#12446=ORIENTED_EDGE('',*,*,#9070,.T.);
#12447=ORIENTED_EDGE('',*,*,#9063,.T.);
#12448=ORIENTED_EDGE('',*,*,#9067,.T.);
#12449=ORIENTED_EDGE('',*,*,#9071,.T.);
#12450=ORIENTED_EDGE('',*,*,#9072,.T.);
#12451=ORIENTED_EDGE('',*,*,#9073,.T.);
#12452=ORIENTED_EDGE('',*,*,#9074,.T.);
#12453=ORIENTED_EDGE('',*,*,#9075,.T.);
#12454=ORIENTED_EDGE('',*,*,#9075,.F.);
#12455=ORIENTED_EDGE('',*,*,#9076,.T.);
#12456=ORIENTED_EDGE('',*,*,#9077,.F.);
#12457=ORIENTED_EDGE('',*,*,#9078,.T.);
#12458=ORIENTED_EDGE('',*,*,#8336,.T.);
#12459=ORIENTED_EDGE('',*,*,#9079,.F.);
#12460=ORIENTED_EDGE('',*,*,#9074,.F.);
#12461=ORIENTED_EDGE('',*,*,#9080,.T.);
#12462=ORIENTED_EDGE('',*,*,#9081,.F.);
#12463=ORIENTED_EDGE('',*,*,#9076,.F.);
#12464=ORIENTED_EDGE('',*,*,#9082,.F.);
#12465=ORIENTED_EDGE('',*,*,#9083,.T.);
#12466=ORIENTED_EDGE('',*,*,#9084,.T.);
#12467=ORIENTED_EDGE('',*,*,#9077,.T.);
#12468=ORIENTED_EDGE('',*,*,#9081,.T.);
#12469=ORIENTED_EDGE('',*,*,#9085,.T.);
#12470=ORIENTED_EDGE('',*,*,#9086,.T.);
#12471=ORIENTED_EDGE('',*,*,#9087,.T.);
#12472=ORIENTED_EDGE('',*,*,#9088,.T.);
#12473=ORIENTED_EDGE('',*,*,#9089,.T.);
#12474=ORIENTED_EDGE('',*,*,#9089,.F.);
#12475=ORIENTED_EDGE('',*,*,#9090,.T.);
#12476=ORIENTED_EDGE('',*,*,#9091,.F.);
#12477=ORIENTED_EDGE('',*,*,#9092,.T.);
#12478=ORIENTED_EDGE('',*,*,#8338,.T.);
#12479=ORIENTED_EDGE('',*,*,#9093,.F.);
#12480=ORIENTED_EDGE('',*,*,#9088,.F.);
#12481=ORIENTED_EDGE('',*,*,#9094,.T.);
#12482=ORIENTED_EDGE('',*,*,#9095,.F.);
#12483=ORIENTED_EDGE('',*,*,#9090,.F.);
#12484=ORIENTED_EDGE('',*,*,#9096,.F.);
#12485=ORIENTED_EDGE('',*,*,#9097,.T.);
#12486=ORIENTED_EDGE('',*,*,#9098,.T.);
#12487=ORIENTED_EDGE('',*,*,#9091,.T.);
#12488=ORIENTED_EDGE('',*,*,#9095,.T.);
#12489=ORIENTED_EDGE('',*,*,#9099,.T.);
#12490=ORIENTED_EDGE('',*,*,#9100,.T.);
#12491=ORIENTED_EDGE('',*,*,#9101,.T.);
#12492=ORIENTED_EDGE('',*,*,#9102,.T.);
#12493=ORIENTED_EDGE('',*,*,#9103,.T.);
#12494=ORIENTED_EDGE('',*,*,#9103,.F.);
#12495=ORIENTED_EDGE('',*,*,#9104,.T.);
#12496=ORIENTED_EDGE('',*,*,#9105,.F.);
#12497=ORIENTED_EDGE('',*,*,#9106,.T.);
#12498=ORIENTED_EDGE('',*,*,#8340,.T.);
#12499=ORIENTED_EDGE('',*,*,#9107,.F.);
#12500=ORIENTED_EDGE('',*,*,#9102,.F.);
#12501=ORIENTED_EDGE('',*,*,#9108,.T.);
#12502=ORIENTED_EDGE('',*,*,#9109,.F.);
#12503=ORIENTED_EDGE('',*,*,#9104,.F.);
#12504=ORIENTED_EDGE('',*,*,#9110,.F.);
#12505=ORIENTED_EDGE('',*,*,#9111,.T.);
#12506=ORIENTED_EDGE('',*,*,#9112,.T.);
#12507=ORIENTED_EDGE('',*,*,#9105,.T.);
#12508=ORIENTED_EDGE('',*,*,#9109,.T.);
#12509=ORIENTED_EDGE('',*,*,#9113,.T.);
#12510=ORIENTED_EDGE('',*,*,#9114,.T.);
#12511=ORIENTED_EDGE('',*,*,#9115,.T.);
#12512=ORIENTED_EDGE('',*,*,#9116,.T.);
#12513=ORIENTED_EDGE('',*,*,#9117,.T.);
#12514=ORIENTED_EDGE('',*,*,#9117,.F.);
#12515=ORIENTED_EDGE('',*,*,#9118,.T.);
#12516=ORIENTED_EDGE('',*,*,#9119,.F.);
#12517=ORIENTED_EDGE('',*,*,#9120,.T.);
#12518=ORIENTED_EDGE('',*,*,#8342,.T.);
#12519=ORIENTED_EDGE('',*,*,#9121,.F.);
#12520=ORIENTED_EDGE('',*,*,#9116,.F.);
#12521=ORIENTED_EDGE('',*,*,#9122,.T.);
#12522=ORIENTED_EDGE('',*,*,#9123,.F.);
#12523=ORIENTED_EDGE('',*,*,#9118,.F.);
#12524=ORIENTED_EDGE('',*,*,#9124,.F.);
#12525=ORIENTED_EDGE('',*,*,#9125,.T.);
#12526=ORIENTED_EDGE('',*,*,#9126,.T.);
#12527=ORIENTED_EDGE('',*,*,#9119,.T.);
#12528=ORIENTED_EDGE('',*,*,#9123,.T.);
#12529=ORIENTED_EDGE('',*,*,#9127,.T.);
#12530=ORIENTED_EDGE('',*,*,#9128,.T.);
#12531=ORIENTED_EDGE('',*,*,#9129,.T.);
#12532=ORIENTED_EDGE('',*,*,#9130,.T.);
#12533=ORIENTED_EDGE('',*,*,#9131,.T.);
#12534=ORIENTED_EDGE('',*,*,#9131,.F.);
#12535=ORIENTED_EDGE('',*,*,#9132,.T.);
#12536=ORIENTED_EDGE('',*,*,#9133,.F.);
#12537=ORIENTED_EDGE('',*,*,#9134,.T.);
#12538=ORIENTED_EDGE('',*,*,#8344,.T.);
#12539=ORIENTED_EDGE('',*,*,#9135,.F.);
#12540=ORIENTED_EDGE('',*,*,#9130,.F.);
#12541=ORIENTED_EDGE('',*,*,#9136,.T.);
#12542=ORIENTED_EDGE('',*,*,#9137,.F.);
#12543=ORIENTED_EDGE('',*,*,#9132,.F.);
#12544=ORIENTED_EDGE('',*,*,#9138,.T.);
#12545=ORIENTED_EDGE('',*,*,#9139,.T.);
#12546=ORIENTED_EDGE('',*,*,#9140,.T.);
#12547=ORIENTED_EDGE('',*,*,#9141,.T.);
#12548=ORIENTED_EDGE('',*,*,#9139,.F.);
#12549=ORIENTED_EDGE('',*,*,#9142,.F.);
#12550=ORIENTED_EDGE('',*,*,#9143,.F.);
#12551=ORIENTED_EDGE('',*,*,#9144,.F.);
#12552=ORIENTED_EDGE('',*,*,#9138,.F.);
#12553=ORIENTED_EDGE('',*,*,#9145,.F.);
#12554=ORIENTED_EDGE('',*,*,#8345,.T.);
#12555=ORIENTED_EDGE('',*,*,#9134,.F.);
#12556=ORIENTED_EDGE('',*,*,#9146,.F.);
#12557=ORIENTED_EDGE('',*,*,#9142,.T.);
#12558=ORIENTED_EDGE('',*,*,#9147,.F.);
#12559=ORIENTED_EDGE('',*,*,#9143,.T.);
#12560=ORIENTED_EDGE('',*,*,#9146,.T.);
#12561=ORIENTED_EDGE('',*,*,#9133,.T.);
#12562=ORIENTED_EDGE('',*,*,#9137,.T.);
#12563=ORIENTED_EDGE('',*,*,#9148,.F.);
#12564=ORIENTED_EDGE('',*,*,#9149,.T.);
#12565=ORIENTED_EDGE('',*,*,#9150,.T.);
#12566=ORIENTED_EDGE('',*,*,#9151,.T.);
#12567=ORIENTED_EDGE('',*,*,#9150,.F.);
#12568=ORIENTED_EDGE('',*,*,#9152,.T.);
#12569=ORIENTED_EDGE('',*,*,#9153,.F.);
#12570=ORIENTED_EDGE('',*,*,#9154,.T.);
#12571=ORIENTED_EDGE('',*,*,#8327,.T.);
#12572=ORIENTED_EDGE('',*,*,#9155,.F.);
#12573=ORIENTED_EDGE('',*,*,#9149,.F.);
#12574=ORIENTED_EDGE('',*,*,#9156,.F.);
#12575=ORIENTED_EDGE('',*,*,#9157,.F.);
#12576=ORIENTED_EDGE('',*,*,#9152,.F.);
#12577=ORIENTED_EDGE('',*,*,#9153,.T.);
#12578=ORIENTED_EDGE('',*,*,#9157,.T.);
#12579=ORIENTED_EDGE('',*,*,#9158,.T.);
#12580=ORIENTED_EDGE('',*,*,#9159,.T.);
#12581=ORIENTED_EDGE('',*,*,#9160,.T.);
#12582=ORIENTED_EDGE('',*,*,#9161,.F.);
#12583=ORIENTED_EDGE('',*,*,#9162,.T.);
#12584=ORIENTED_EDGE('',*,*,#9163,.T.);
#12585=ORIENTED_EDGE('',*,*,#9164,.T.);
#12586=ORIENTED_EDGE('',*,*,#9165,.T.);
#12587=ORIENTED_EDGE('',*,*,#9163,.F.);
#12588=ORIENTED_EDGE('',*,*,#9166,.T.);
#12589=ORIENTED_EDGE('',*,*,#9167,.F.);
#12590=ORIENTED_EDGE('',*,*,#9168,.F.);
#12591=ORIENTED_EDGE('',*,*,#8329,.T.);
#12592=ORIENTED_EDGE('',*,*,#9169,.F.);
#12593=ORIENTED_EDGE('',*,*,#9162,.F.);
#12594=ORIENTED_EDGE('',*,*,#9170,.F.);
#12595=ORIENTED_EDGE('',*,*,#9171,.F.);
#12596=ORIENTED_EDGE('',*,*,#9166,.F.);
#12597=ORIENTED_EDGE('',*,*,#9172,.T.);
#12598=ORIENTED_EDGE('',*,*,#9173,.F.);
#12599=ORIENTED_EDGE('',*,*,#9174,.T.);
#12600=ORIENTED_EDGE('',*,*,#9175,.T.);
#12601=ORIENTED_EDGE('',*,*,#9043,.F.);
#12602=ORIENTED_EDGE('',*,*,#9051,.T.);
#12603=ORIENTED_EDGE('',*,*,#8331,.T.);
#12604=ORIENTED_EDGE('',*,*,#9176,.T.);
#12605=ORIENTED_EDGE('',*,*,#9175,.F.);
#12606=ORIENTED_EDGE('',*,*,#9177,.T.);
#12607=ORIENTED_EDGE('',*,*,#9056,.F.);
#12608=ORIENTED_EDGE('',*,*,#9178,.T.);
#12609=ORIENTED_EDGE('',*,*,#9057,.F.);
#12610=ORIENTED_EDGE('',*,*,#9065,.T.);
#12611=ORIENTED_EDGE('',*,*,#8333,.T.);
#12612=ORIENTED_EDGE('',*,*,#9050,.F.);
#12613=ORIENTED_EDGE('',*,*,#9070,.F.);
#12614=ORIENTED_EDGE('',*,*,#9179,.T.);
#12615=ORIENTED_EDGE('',*,*,#9071,.F.);
#12616=ORIENTED_EDGE('',*,*,#9079,.T.);
#12617=ORIENTED_EDGE('',*,*,#8335,.T.);
#12618=ORIENTED_EDGE('',*,*,#9064,.F.);
#12619=ORIENTED_EDGE('',*,*,#9084,.F.);
#12620=ORIENTED_EDGE('',*,*,#9180,.T.);
#12621=ORIENTED_EDGE('',*,*,#9085,.F.);
#12622=ORIENTED_EDGE('',*,*,#9093,.T.);
#12623=ORIENTED_EDGE('',*,*,#8337,.T.);
#12624=ORIENTED_EDGE('',*,*,#9078,.F.);
#12625=ORIENTED_EDGE('',*,*,#9098,.F.);
#12626=ORIENTED_EDGE('',*,*,#9181,.T.);
#12627=ORIENTED_EDGE('',*,*,#9099,.F.);
#12628=ORIENTED_EDGE('',*,*,#9107,.T.);
#12629=ORIENTED_EDGE('',*,*,#8339,.T.);
#12630=ORIENTED_EDGE('',*,*,#9092,.F.);
#12631=ORIENTED_EDGE('',*,*,#9112,.F.);
#12632=ORIENTED_EDGE('',*,*,#9182,.T.);
#12633=ORIENTED_EDGE('',*,*,#9113,.F.);
#12634=ORIENTED_EDGE('',*,*,#9121,.T.);
#12635=ORIENTED_EDGE('',*,*,#8341,.T.);
#12636=ORIENTED_EDGE('',*,*,#9106,.F.);
#12637=ORIENTED_EDGE('',*,*,#9126,.F.);
#12638=ORIENTED_EDGE('',*,*,#9183,.T.);
#12639=ORIENTED_EDGE('',*,*,#9127,.F.);
#12640=ORIENTED_EDGE('',*,*,#9135,.T.);
#12641=ORIENTED_EDGE('',*,*,#8343,.T.);
#12642=ORIENTED_EDGE('',*,*,#9120,.F.);
#12643=ORIENTED_EDGE('',*,*,#9125,.F.);
#12644=ORIENTED_EDGE('',*,*,#9184,.F.);
#12645=ORIENTED_EDGE('',*,*,#9128,.F.);
#12646=ORIENTED_EDGE('',*,*,#9183,.F.);
#12647=ORIENTED_EDGE('',*,*,#9111,.F.);
#12648=ORIENTED_EDGE('',*,*,#9185,.F.);
#12649=ORIENTED_EDGE('',*,*,#9114,.F.);
#12650=ORIENTED_EDGE('',*,*,#9182,.F.);
#12651=ORIENTED_EDGE('',*,*,#9097,.F.);
#12652=ORIENTED_EDGE('',*,*,#9186,.F.);
#12653=ORIENTED_EDGE('',*,*,#9100,.F.);
#12654=ORIENTED_EDGE('',*,*,#9181,.F.);
#12655=ORIENTED_EDGE('',*,*,#9083,.F.);
#12656=ORIENTED_EDGE('',*,*,#9187,.F.);
#12657=ORIENTED_EDGE('',*,*,#9086,.F.);
#12658=ORIENTED_EDGE('',*,*,#9180,.F.);
#12659=ORIENTED_EDGE('',*,*,#9069,.F.);
#12660=ORIENTED_EDGE('',*,*,#9188,.F.);
#12661=ORIENTED_EDGE('',*,*,#9072,.F.);
#12662=ORIENTED_EDGE('',*,*,#9179,.F.);
#12663=ORIENTED_EDGE('',*,*,#9055,.F.);
#12664=ORIENTED_EDGE('',*,*,#9189,.F.);
#12665=ORIENTED_EDGE('',*,*,#9058,.F.);
#12666=ORIENTED_EDGE('',*,*,#9178,.F.);
#12667=ORIENTED_EDGE('',*,*,#9044,.F.);
#12668=ORIENTED_EDGE('',*,*,#9177,.F.);
#12669=ORIENTED_EDGE('',*,*,#9174,.F.);
#12670=ORIENTED_EDGE('',*,*,#9190,.F.);
#12671=ORIENTED_EDGE('',*,*,#9167,.T.);
#12672=ORIENTED_EDGE('',*,*,#9171,.T.);
#12673=ORIENTED_EDGE('',*,*,#9191,.T.);
#12674=ORIENTED_EDGE('',*,*,#9192,.T.);
#12675=ORIENTED_EDGE('',*,*,#9160,.F.);
#12676=ORIENTED_EDGE('',*,*,#9193,.T.);
#12677=ORIENTED_EDGE('',*,*,#9164,.F.);
#12678=ORIENTED_EDGE('',*,*,#9169,.T.);
#12679=ORIENTED_EDGE('',*,*,#8328,.T.);
#12680=ORIENTED_EDGE('',*,*,#9154,.F.);
#12681=ORIENTED_EDGE('',*,*,#9176,.F.);
#12682=ORIENTED_EDGE('',*,*,#8330,.F.);
#12683=ORIENTED_EDGE('',*,*,#9168,.T.);
#12684=ORIENTED_EDGE('',*,*,#9192,.F.);
#12685=ORIENTED_EDGE('',*,*,#9194,.T.);
#12686=ORIENTED_EDGE('',*,*,#9172,.F.);
#12687=ORIENTED_EDGE('',*,*,#9159,.F.);
#12688=ORIENTED_EDGE('',*,*,#9195,.T.);
#12689=ORIENTED_EDGE('',*,*,#9165,.F.);
#12690=ORIENTED_EDGE('',*,*,#9193,.F.);
#12691=ORIENTED_EDGE('',*,*,#9196,.T.);
#12692=ORIENTED_EDGE('',*,*,#9197,.T.);
#12693=ORIENTED_EDGE('',*,*,#9198,.T.);
#12694=ORIENTED_EDGE('',*,*,#9199,.T.);
#12695=ORIENTED_EDGE('',*,*,#9200,.T.);
#12696=ORIENTED_EDGE('',*,*,#9200,.F.);
#12697=ORIENTED_EDGE('',*,*,#9201,.T.);
#12698=ORIENTED_EDGE('',*,*,#9202,.F.);
#12699=ORIENTED_EDGE('',*,*,#9203,.T.);
#12700=ORIENTED_EDGE('',*,*,#8310,.T.);
#12701=ORIENTED_EDGE('',*,*,#9204,.F.);
#12702=ORIENTED_EDGE('',*,*,#9199,.F.);
#12703=ORIENTED_EDGE('',*,*,#9205,.T.);
#12704=ORIENTED_EDGE('',*,*,#9206,.F.);
#12705=ORIENTED_EDGE('',*,*,#9201,.F.);
#12706=ORIENTED_EDGE('',*,*,#9207,.F.);
#12707=ORIENTED_EDGE('',*,*,#9208,.T.);
#12708=ORIENTED_EDGE('',*,*,#9209,.T.);
#12709=ORIENTED_EDGE('',*,*,#9202,.T.);
#12710=ORIENTED_EDGE('',*,*,#9206,.T.);
#12711=ORIENTED_EDGE('',*,*,#9210,.T.);
#12712=ORIENTED_EDGE('',*,*,#9211,.T.);
#12713=ORIENTED_EDGE('',*,*,#9212,.T.);
#12714=ORIENTED_EDGE('',*,*,#9213,.T.);
#12715=ORIENTED_EDGE('',*,*,#9214,.T.);
#12716=ORIENTED_EDGE('',*,*,#9214,.F.);
#12717=ORIENTED_EDGE('',*,*,#9215,.T.);
#12718=ORIENTED_EDGE('',*,*,#9216,.F.);
#12719=ORIENTED_EDGE('',*,*,#9217,.T.);
#12720=ORIENTED_EDGE('',*,*,#8312,.T.);
#12721=ORIENTED_EDGE('',*,*,#9218,.F.);
#12722=ORIENTED_EDGE('',*,*,#9213,.F.);
#12723=ORIENTED_EDGE('',*,*,#9219,.T.);
#12724=ORIENTED_EDGE('',*,*,#9220,.F.);
#12725=ORIENTED_EDGE('',*,*,#9215,.F.);
#12726=ORIENTED_EDGE('',*,*,#9221,.F.);
#12727=ORIENTED_EDGE('',*,*,#9222,.T.);
#12728=ORIENTED_EDGE('',*,*,#9223,.T.);
#12729=ORIENTED_EDGE('',*,*,#9216,.T.);
#12730=ORIENTED_EDGE('',*,*,#9220,.T.);
#12731=ORIENTED_EDGE('',*,*,#9224,.T.);
#12732=ORIENTED_EDGE('',*,*,#9225,.T.);
#12733=ORIENTED_EDGE('',*,*,#9226,.T.);
#12734=ORIENTED_EDGE('',*,*,#9227,.T.);
#12735=ORIENTED_EDGE('',*,*,#9228,.T.);
#12736=ORIENTED_EDGE('',*,*,#9228,.F.);
#12737=ORIENTED_EDGE('',*,*,#9229,.T.);
#12738=ORIENTED_EDGE('',*,*,#9230,.F.);
#12739=ORIENTED_EDGE('',*,*,#9231,.T.);
#12740=ORIENTED_EDGE('',*,*,#8314,.T.);
#12741=ORIENTED_EDGE('',*,*,#9232,.F.);
#12742=ORIENTED_EDGE('',*,*,#9227,.F.);
#12743=ORIENTED_EDGE('',*,*,#9233,.T.);
#12744=ORIENTED_EDGE('',*,*,#9234,.F.);
#12745=ORIENTED_EDGE('',*,*,#9229,.F.);
#12746=ORIENTED_EDGE('',*,*,#9235,.F.);
#12747=ORIENTED_EDGE('',*,*,#9236,.T.);
#12748=ORIENTED_EDGE('',*,*,#9237,.T.);
#12749=ORIENTED_EDGE('',*,*,#9230,.T.);
#12750=ORIENTED_EDGE('',*,*,#9234,.T.);
#12751=ORIENTED_EDGE('',*,*,#9238,.T.);
#12752=ORIENTED_EDGE('',*,*,#9239,.T.);
#12753=ORIENTED_EDGE('',*,*,#9240,.T.);
#12754=ORIENTED_EDGE('',*,*,#9241,.T.);
#12755=ORIENTED_EDGE('',*,*,#9242,.T.);
#12756=ORIENTED_EDGE('',*,*,#9242,.F.);
#12757=ORIENTED_EDGE('',*,*,#9243,.T.);
#12758=ORIENTED_EDGE('',*,*,#9244,.F.);
#12759=ORIENTED_EDGE('',*,*,#9245,.T.);
#12760=ORIENTED_EDGE('',*,*,#8316,.T.);
#12761=ORIENTED_EDGE('',*,*,#9246,.F.);
#12762=ORIENTED_EDGE('',*,*,#9241,.F.);
#12763=ORIENTED_EDGE('',*,*,#9247,.T.);
#12764=ORIENTED_EDGE('',*,*,#9248,.F.);
#12765=ORIENTED_EDGE('',*,*,#9243,.F.);
#12766=ORIENTED_EDGE('',*,*,#9249,.F.);
#12767=ORIENTED_EDGE('',*,*,#9250,.T.);
#12768=ORIENTED_EDGE('',*,*,#9251,.T.);
#12769=ORIENTED_EDGE('',*,*,#9244,.T.);
#12770=ORIENTED_EDGE('',*,*,#9248,.T.);
#12771=ORIENTED_EDGE('',*,*,#9252,.T.);
#12772=ORIENTED_EDGE('',*,*,#9253,.T.);
#12773=ORIENTED_EDGE('',*,*,#9254,.T.);
#12774=ORIENTED_EDGE('',*,*,#9255,.T.);
#12775=ORIENTED_EDGE('',*,*,#9256,.T.);
#12776=ORIENTED_EDGE('',*,*,#9256,.F.);
#12777=ORIENTED_EDGE('',*,*,#9257,.T.);
#12778=ORIENTED_EDGE('',*,*,#9258,.F.);
#12779=ORIENTED_EDGE('',*,*,#9259,.T.);
#12780=ORIENTED_EDGE('',*,*,#8318,.T.);
#12781=ORIENTED_EDGE('',*,*,#9260,.F.);
#12782=ORIENTED_EDGE('',*,*,#9255,.F.);
#12783=ORIENTED_EDGE('',*,*,#9261,.T.);
#12784=ORIENTED_EDGE('',*,*,#9262,.F.);
#12785=ORIENTED_EDGE('',*,*,#9257,.F.);
#12786=ORIENTED_EDGE('',*,*,#9263,.F.);
#12787=ORIENTED_EDGE('',*,*,#9264,.T.);
#12788=ORIENTED_EDGE('',*,*,#9265,.T.);
#12789=ORIENTED_EDGE('',*,*,#9258,.T.);
#12790=ORIENTED_EDGE('',*,*,#9262,.T.);
#12791=ORIENTED_EDGE('',*,*,#9266,.T.);
#12792=ORIENTED_EDGE('',*,*,#9267,.T.);
#12793=ORIENTED_EDGE('',*,*,#9268,.T.);
#12794=ORIENTED_EDGE('',*,*,#9269,.T.);
#12795=ORIENTED_EDGE('',*,*,#9270,.T.);
#12796=ORIENTED_EDGE('',*,*,#9270,.F.);
#12797=ORIENTED_EDGE('',*,*,#9271,.T.);
#12798=ORIENTED_EDGE('',*,*,#9272,.F.);
#12799=ORIENTED_EDGE('',*,*,#9273,.T.);
#12800=ORIENTED_EDGE('',*,*,#8320,.T.);
#12801=ORIENTED_EDGE('',*,*,#9274,.F.);
#12802=ORIENTED_EDGE('',*,*,#9269,.F.);
#12803=ORIENTED_EDGE('',*,*,#9275,.T.);
#12804=ORIENTED_EDGE('',*,*,#9276,.F.);
#12805=ORIENTED_EDGE('',*,*,#9271,.F.);
#12806=ORIENTED_EDGE('',*,*,#9277,.F.);
#12807=ORIENTED_EDGE('',*,*,#9278,.T.);
#12808=ORIENTED_EDGE('',*,*,#9279,.T.);
#12809=ORIENTED_EDGE('',*,*,#9272,.T.);
#12810=ORIENTED_EDGE('',*,*,#9276,.T.);
#12811=ORIENTED_EDGE('',*,*,#9280,.T.);
#12812=ORIENTED_EDGE('',*,*,#9281,.T.);
#12813=ORIENTED_EDGE('',*,*,#9282,.T.);
#12814=ORIENTED_EDGE('',*,*,#9283,.T.);
#12815=ORIENTED_EDGE('',*,*,#9284,.T.);
#12816=ORIENTED_EDGE('',*,*,#9284,.F.);
#12817=ORIENTED_EDGE('',*,*,#9285,.T.);
#12818=ORIENTED_EDGE('',*,*,#9286,.F.);
#12819=ORIENTED_EDGE('',*,*,#9287,.T.);
#12820=ORIENTED_EDGE('',*,*,#8322,.T.);
#12821=ORIENTED_EDGE('',*,*,#9288,.F.);
#12822=ORIENTED_EDGE('',*,*,#9283,.F.);
#12823=ORIENTED_EDGE('',*,*,#9289,.T.);
#12824=ORIENTED_EDGE('',*,*,#9290,.F.);
#12825=ORIENTED_EDGE('',*,*,#9285,.F.);
#12826=ORIENTED_EDGE('',*,*,#9291,.F.);
#12827=ORIENTED_EDGE('',*,*,#9292,.T.);
#12828=ORIENTED_EDGE('',*,*,#9293,.T.);
#12829=ORIENTED_EDGE('',*,*,#9286,.T.);
#12830=ORIENTED_EDGE('',*,*,#9290,.T.);
#12831=ORIENTED_EDGE('',*,*,#9294,.T.);
#12832=ORIENTED_EDGE('',*,*,#9295,.T.);
#12833=ORIENTED_EDGE('',*,*,#9296,.T.);
#12834=ORIENTED_EDGE('',*,*,#9297,.T.);
#12835=ORIENTED_EDGE('',*,*,#9298,.T.);
#12836=ORIENTED_EDGE('',*,*,#9298,.F.);
#12837=ORIENTED_EDGE('',*,*,#9299,.T.);
#12838=ORIENTED_EDGE('',*,*,#9300,.F.);
#12839=ORIENTED_EDGE('',*,*,#9301,.T.);
#12840=ORIENTED_EDGE('',*,*,#8324,.T.);
#12841=ORIENTED_EDGE('',*,*,#9302,.F.);
#12842=ORIENTED_EDGE('',*,*,#9297,.F.);
#12843=ORIENTED_EDGE('',*,*,#9303,.T.);
#12844=ORIENTED_EDGE('',*,*,#9304,.F.);
#12845=ORIENTED_EDGE('',*,*,#9299,.F.);
#12846=ORIENTED_EDGE('',*,*,#9305,.T.);
#12847=ORIENTED_EDGE('',*,*,#9306,.T.);
#12848=ORIENTED_EDGE('',*,*,#9307,.T.);
#12849=ORIENTED_EDGE('',*,*,#9308,.T.);
#12850=ORIENTED_EDGE('',*,*,#9306,.F.);
#12851=ORIENTED_EDGE('',*,*,#9309,.F.);
#12852=ORIENTED_EDGE('',*,*,#9310,.F.);
#12853=ORIENTED_EDGE('',*,*,#9311,.F.);
#12854=ORIENTED_EDGE('',*,*,#9305,.F.);
#12855=ORIENTED_EDGE('',*,*,#9312,.F.);
#12856=ORIENTED_EDGE('',*,*,#8325,.T.);
#12857=ORIENTED_EDGE('',*,*,#9301,.F.);
#12858=ORIENTED_EDGE('',*,*,#9313,.F.);
#12859=ORIENTED_EDGE('',*,*,#9309,.T.);
#12860=ORIENTED_EDGE('',*,*,#9314,.F.);
#12861=ORIENTED_EDGE('',*,*,#9310,.T.);
#12862=ORIENTED_EDGE('',*,*,#9313,.T.);
#12863=ORIENTED_EDGE('',*,*,#9300,.T.);
#12864=ORIENTED_EDGE('',*,*,#9304,.T.);
#12865=ORIENTED_EDGE('',*,*,#9315,.F.);
#12866=ORIENTED_EDGE('',*,*,#9316,.T.);
#12867=ORIENTED_EDGE('',*,*,#9317,.T.);
#12868=ORIENTED_EDGE('',*,*,#9318,.T.);
#12869=ORIENTED_EDGE('',*,*,#9317,.F.);
#12870=ORIENTED_EDGE('',*,*,#9319,.T.);
#12871=ORIENTED_EDGE('',*,*,#9320,.F.);
#12872=ORIENTED_EDGE('',*,*,#9321,.F.);
#12873=ORIENTED_EDGE('',*,*,#8307,.T.);
#12874=ORIENTED_EDGE('',*,*,#9322,.F.);
#12875=ORIENTED_EDGE('',*,*,#9316,.F.);
#12876=ORIENTED_EDGE('',*,*,#9323,.F.);
#12877=ORIENTED_EDGE('',*,*,#9324,.F.);
#12878=ORIENTED_EDGE('',*,*,#9319,.F.);
#12879=ORIENTED_EDGE('',*,*,#9325,.T.);
#12880=ORIENTED_EDGE('',*,*,#9326,.F.);
#12881=ORIENTED_EDGE('',*,*,#9327,.T.);
#12882=ORIENTED_EDGE('',*,*,#9328,.T.);
#12883=ORIENTED_EDGE('',*,*,#9196,.F.);
#12884=ORIENTED_EDGE('',*,*,#9204,.T.);
#12885=ORIENTED_EDGE('',*,*,#8309,.T.);
#12886=ORIENTED_EDGE('',*,*,#9329,.T.);
#12887=ORIENTED_EDGE('',*,*,#9328,.F.);
#12888=ORIENTED_EDGE('',*,*,#9330,.T.);
#12889=ORIENTED_EDGE('',*,*,#9209,.F.);
#12890=ORIENTED_EDGE('',*,*,#9331,.T.);
#12891=ORIENTED_EDGE('',*,*,#9210,.F.);
#12892=ORIENTED_EDGE('',*,*,#9218,.T.);
#12893=ORIENTED_EDGE('',*,*,#8311,.T.);
#12894=ORIENTED_EDGE('',*,*,#9203,.F.);
#12895=ORIENTED_EDGE('',*,*,#9223,.F.);
#12896=ORIENTED_EDGE('',*,*,#9332,.T.);
#12897=ORIENTED_EDGE('',*,*,#9224,.F.);
#12898=ORIENTED_EDGE('',*,*,#9232,.T.);
#12899=ORIENTED_EDGE('',*,*,#8313,.T.);
#12900=ORIENTED_EDGE('',*,*,#9217,.F.);
#12901=ORIENTED_EDGE('',*,*,#9237,.F.);
#12902=ORIENTED_EDGE('',*,*,#9333,.T.);
#12903=ORIENTED_EDGE('',*,*,#9238,.F.);
#12904=ORIENTED_EDGE('',*,*,#9246,.T.);
#12905=ORIENTED_EDGE('',*,*,#8315,.T.);
#12906=ORIENTED_EDGE('',*,*,#9231,.F.);
#12907=ORIENTED_EDGE('',*,*,#9251,.F.);
#12908=ORIENTED_EDGE('',*,*,#9334,.T.);
#12909=ORIENTED_EDGE('',*,*,#9252,.F.);
#12910=ORIENTED_EDGE('',*,*,#9260,.T.);
#12911=ORIENTED_EDGE('',*,*,#8317,.T.);
#12912=ORIENTED_EDGE('',*,*,#9245,.F.);
#12913=ORIENTED_EDGE('',*,*,#9265,.F.);
#12914=ORIENTED_EDGE('',*,*,#9335,.T.);
#12915=ORIENTED_EDGE('',*,*,#9266,.F.);
#12916=ORIENTED_EDGE('',*,*,#9274,.T.);
#12917=ORIENTED_EDGE('',*,*,#8319,.T.);
#12918=ORIENTED_EDGE('',*,*,#9259,.F.);
#12919=ORIENTED_EDGE('',*,*,#9279,.F.);
#12920=ORIENTED_EDGE('',*,*,#9336,.T.);
#12921=ORIENTED_EDGE('',*,*,#9280,.F.);
#12922=ORIENTED_EDGE('',*,*,#9288,.T.);
#12923=ORIENTED_EDGE('',*,*,#8321,.T.);
#12924=ORIENTED_EDGE('',*,*,#9273,.F.);
#12925=ORIENTED_EDGE('',*,*,#9293,.F.);
#12926=ORIENTED_EDGE('',*,*,#9337,.T.);
#12927=ORIENTED_EDGE('',*,*,#9294,.F.);
#12928=ORIENTED_EDGE('',*,*,#9302,.T.);
#12929=ORIENTED_EDGE('',*,*,#8323,.T.);
#12930=ORIENTED_EDGE('',*,*,#9287,.F.);
#12931=ORIENTED_EDGE('',*,*,#9292,.F.);
#12932=ORIENTED_EDGE('',*,*,#9338,.F.);
#12933=ORIENTED_EDGE('',*,*,#9295,.F.);
#12934=ORIENTED_EDGE('',*,*,#9337,.F.);
#12935=ORIENTED_EDGE('',*,*,#9278,.F.);
#12936=ORIENTED_EDGE('',*,*,#9339,.F.);
#12937=ORIENTED_EDGE('',*,*,#9281,.F.);
#12938=ORIENTED_EDGE('',*,*,#9336,.F.);
#12939=ORIENTED_EDGE('',*,*,#9264,.F.);
#12940=ORIENTED_EDGE('',*,*,#9340,.F.);
#12941=ORIENTED_EDGE('',*,*,#9267,.F.);
#12942=ORIENTED_EDGE('',*,*,#9335,.F.);
#12943=ORIENTED_EDGE('',*,*,#9250,.F.);
#12944=ORIENTED_EDGE('',*,*,#9341,.F.);
#12945=ORIENTED_EDGE('',*,*,#9253,.F.);
#12946=ORIENTED_EDGE('',*,*,#9334,.F.);
#12947=ORIENTED_EDGE('',*,*,#9236,.F.);
#12948=ORIENTED_EDGE('',*,*,#9342,.F.);
#12949=ORIENTED_EDGE('',*,*,#9239,.F.);
#12950=ORIENTED_EDGE('',*,*,#9333,.F.);
#12951=ORIENTED_EDGE('',*,*,#9222,.F.);
#12952=ORIENTED_EDGE('',*,*,#9343,.F.);
#12953=ORIENTED_EDGE('',*,*,#9225,.F.);
#12954=ORIENTED_EDGE('',*,*,#9332,.F.);
#12955=ORIENTED_EDGE('',*,*,#9208,.F.);
#12956=ORIENTED_EDGE('',*,*,#9344,.F.);
#12957=ORIENTED_EDGE('',*,*,#9211,.F.);
#12958=ORIENTED_EDGE('',*,*,#9331,.F.);
#12959=ORIENTED_EDGE('',*,*,#9197,.F.);
#12960=ORIENTED_EDGE('',*,*,#9330,.F.);
#12961=ORIENTED_EDGE('',*,*,#9327,.F.);
#12962=ORIENTED_EDGE('',*,*,#9345,.F.);
#12963=ORIENTED_EDGE('',*,*,#9320,.T.);
#12964=ORIENTED_EDGE('',*,*,#9324,.T.);
#12965=ORIENTED_EDGE('',*,*,#9346,.T.);
#12966=ORIENTED_EDGE('',*,*,#9347,.T.);
#12967=ORIENTED_EDGE('',*,*,#9329,.F.);
#12968=ORIENTED_EDGE('',*,*,#8308,.F.);
#12969=ORIENTED_EDGE('',*,*,#9321,.T.);
#12970=ORIENTED_EDGE('',*,*,#9347,.F.);
#12971=ORIENTED_EDGE('',*,*,#9348,.T.);
#12972=ORIENTED_EDGE('',*,*,#9325,.F.);
#12973=ORIENTED_EDGE('',*,*,#9349,.F.);
#12974=ORIENTED_EDGE('',*,*,#9350,.T.);
#12975=ORIENTED_EDGE('',*,*,#9351,.T.);
#12976=ORIENTED_EDGE('',*,*,#8256,.T.);
#12977=ORIENTED_EDGE('',*,*,#9352,.T.);
#12978=ORIENTED_EDGE('',*,*,#9351,.F.);
#12979=ORIENTED_EDGE('',*,*,#9353,.T.);
#12980=ORIENTED_EDGE('',*,*,#9354,.F.);
#12981=ORIENTED_EDGE('',*,*,#9355,.T.);
#12982=ORIENTED_EDGE('',*,*,#8288,.T.);
#12983=ORIENTED_EDGE('',*,*,#8257,.T.);
#12984=ORIENTED_EDGE('',*,*,#9350,.F.);
#12985=ORIENTED_EDGE('',*,*,#9356,.F.);
#12986=ORIENTED_EDGE('',*,*,#9357,.F.);
#12987=ORIENTED_EDGE('',*,*,#9353,.F.);
#12988=ORIENTED_EDGE('',*,*,#9354,.T.);
#12989=ORIENTED_EDGE('',*,*,#9357,.T.);
#12990=ORIENTED_EDGE('',*,*,#9358,.T.);
#12991=ORIENTED_EDGE('',*,*,#9359,.T.);
#12992=ORIENTED_EDGE('',*,*,#9360,.T.);
#12993=ORIENTED_EDGE('',*,*,#9361,.F.);
#12994=ORIENTED_EDGE('',*,*,#9362,.T.);
#12995=ORIENTED_EDGE('',*,*,#9363,.T.);
#12996=ORIENTED_EDGE('',*,*,#9364,.T.);
#12997=ORIENTED_EDGE('',*,*,#9365,.T.);
#12998=ORIENTED_EDGE('',*,*,#9363,.F.);
#12999=ORIENTED_EDGE('',*,*,#9366,.T.);
#13000=ORIENTED_EDGE('',*,*,#9367,.F.);
#13001=ORIENTED_EDGE('',*,*,#9368,.T.);
#13002=ORIENTED_EDGE('',*,*,#8290,.T.);
#13003=ORIENTED_EDGE('',*,*,#9369,.F.);
#13004=ORIENTED_EDGE('',*,*,#9362,.F.);
#13005=ORIENTED_EDGE('',*,*,#9370,.F.);
#13006=ORIENTED_EDGE('',*,*,#9371,.F.);
#13007=ORIENTED_EDGE('',*,*,#9366,.F.);
#13008=ORIENTED_EDGE('',*,*,#9367,.T.);
#13009=ORIENTED_EDGE('',*,*,#9371,.T.);
#13010=ORIENTED_EDGE('',*,*,#9372,.T.);
#13011=ORIENTED_EDGE('',*,*,#9373,.T.);
#13012=ORIENTED_EDGE('',*,*,#9374,.T.);
#13013=ORIENTED_EDGE('',*,*,#9375,.F.);
#13014=ORIENTED_EDGE('',*,*,#9376,.T.);
#13015=ORIENTED_EDGE('',*,*,#9377,.T.);
#13016=ORIENTED_EDGE('',*,*,#9378,.T.);
#13017=ORIENTED_EDGE('',*,*,#9379,.T.);
#13018=ORIENTED_EDGE('',*,*,#9377,.F.);
#13019=ORIENTED_EDGE('',*,*,#9380,.T.);
#13020=ORIENTED_EDGE('',*,*,#9381,.F.);
#13021=ORIENTED_EDGE('',*,*,#9382,.T.);
#13022=ORIENTED_EDGE('',*,*,#8292,.T.);
#13023=ORIENTED_EDGE('',*,*,#9383,.F.);
#13024=ORIENTED_EDGE('',*,*,#9376,.F.);
#13025=ORIENTED_EDGE('',*,*,#9384,.F.);
#13026=ORIENTED_EDGE('',*,*,#9385,.F.);
#13027=ORIENTED_EDGE('',*,*,#9380,.F.);
#13028=ORIENTED_EDGE('',*,*,#9381,.T.);
#13029=ORIENTED_EDGE('',*,*,#9385,.T.);
#13030=ORIENTED_EDGE('',*,*,#9386,.T.);
#13031=ORIENTED_EDGE('',*,*,#9387,.T.);
#13032=ORIENTED_EDGE('',*,*,#9388,.T.);
#13033=ORIENTED_EDGE('',*,*,#9389,.F.);
#13034=ORIENTED_EDGE('',*,*,#9390,.T.);
#13035=ORIENTED_EDGE('',*,*,#9391,.T.);
#13036=ORIENTED_EDGE('',*,*,#9392,.T.);
#13037=ORIENTED_EDGE('',*,*,#9393,.T.);
#13038=ORIENTED_EDGE('',*,*,#9391,.F.);
#13039=ORIENTED_EDGE('',*,*,#9394,.T.);
#13040=ORIENTED_EDGE('',*,*,#9395,.F.);
#13041=ORIENTED_EDGE('',*,*,#9396,.T.);
#13042=ORIENTED_EDGE('',*,*,#8294,.T.);
#13043=ORIENTED_EDGE('',*,*,#9397,.F.);
#13044=ORIENTED_EDGE('',*,*,#9390,.F.);
#13045=ORIENTED_EDGE('',*,*,#9398,.F.);
#13046=ORIENTED_EDGE('',*,*,#9399,.F.);
#13047=ORIENTED_EDGE('',*,*,#9394,.F.);
#13048=ORIENTED_EDGE('',*,*,#9395,.T.);
#13049=ORIENTED_EDGE('',*,*,#9399,.T.);
#13050=ORIENTED_EDGE('',*,*,#9400,.T.);
#13051=ORIENTED_EDGE('',*,*,#9401,.T.);
#13052=ORIENTED_EDGE('',*,*,#9402,.T.);
#13053=ORIENTED_EDGE('',*,*,#9403,.F.);
#13054=ORIENTED_EDGE('',*,*,#9404,.T.);
#13055=ORIENTED_EDGE('',*,*,#9405,.T.);
#13056=ORIENTED_EDGE('',*,*,#9406,.T.);
#13057=ORIENTED_EDGE('',*,*,#9407,.T.);
#13058=ORIENTED_EDGE('',*,*,#9405,.F.);
#13059=ORIENTED_EDGE('',*,*,#9408,.T.);
#13060=ORIENTED_EDGE('',*,*,#9409,.F.);
#13061=ORIENTED_EDGE('',*,*,#9410,.T.);
#13062=ORIENTED_EDGE('',*,*,#8296,.T.);
#13063=ORIENTED_EDGE('',*,*,#9411,.F.);
#13064=ORIENTED_EDGE('',*,*,#9404,.F.);
#13065=ORIENTED_EDGE('',*,*,#9412,.F.);
#13066=ORIENTED_EDGE('',*,*,#9413,.F.);
#13067=ORIENTED_EDGE('',*,*,#9408,.F.);
#13068=ORIENTED_EDGE('',*,*,#9409,.T.);
#13069=ORIENTED_EDGE('',*,*,#9413,.T.);
#13070=ORIENTED_EDGE('',*,*,#9414,.T.);
#13071=ORIENTED_EDGE('',*,*,#9415,.T.);
#13072=ORIENTED_EDGE('',*,*,#9416,.T.);
#13073=ORIENTED_EDGE('',*,*,#9417,.F.);
#13074=ORIENTED_EDGE('',*,*,#9418,.T.);
#13075=ORIENTED_EDGE('',*,*,#9419,.T.);
#13076=ORIENTED_EDGE('',*,*,#9420,.T.);
#13077=ORIENTED_EDGE('',*,*,#9421,.T.);
#13078=ORIENTED_EDGE('',*,*,#9419,.F.);
#13079=ORIENTED_EDGE('',*,*,#9422,.T.);
#13080=ORIENTED_EDGE('',*,*,#9423,.F.);
#13081=ORIENTED_EDGE('',*,*,#9424,.T.);
#13082=ORIENTED_EDGE('',*,*,#8298,.T.);
#13083=ORIENTED_EDGE('',*,*,#9425,.F.);
#13084=ORIENTED_EDGE('',*,*,#9418,.F.);
#13085=ORIENTED_EDGE('',*,*,#9426,.F.);
#13086=ORIENTED_EDGE('',*,*,#9427,.F.);
#13087=ORIENTED_EDGE('',*,*,#9422,.F.);
#13088=ORIENTED_EDGE('',*,*,#9423,.T.);
#13089=ORIENTED_EDGE('',*,*,#9427,.T.);
#13090=ORIENTED_EDGE('',*,*,#9428,.T.);
#13091=ORIENTED_EDGE('',*,*,#9429,.T.);
#13092=ORIENTED_EDGE('',*,*,#9430,.T.);
#13093=ORIENTED_EDGE('',*,*,#9431,.F.);
#13094=ORIENTED_EDGE('',*,*,#9432,.T.);
#13095=ORIENTED_EDGE('',*,*,#9433,.T.);
#13096=ORIENTED_EDGE('',*,*,#9434,.T.);
#13097=ORIENTED_EDGE('',*,*,#9435,.T.);
#13098=ORIENTED_EDGE('',*,*,#9433,.F.);
#13099=ORIENTED_EDGE('',*,*,#9436,.T.);
#13100=ORIENTED_EDGE('',*,*,#9437,.F.);
#13101=ORIENTED_EDGE('',*,*,#9438,.T.);
#13102=ORIENTED_EDGE('',*,*,#8300,.T.);
#13103=ORIENTED_EDGE('',*,*,#9439,.F.);
#13104=ORIENTED_EDGE('',*,*,#9432,.F.);
#13105=ORIENTED_EDGE('',*,*,#9440,.F.);
#13106=ORIENTED_EDGE('',*,*,#9441,.F.);
#13107=ORIENTED_EDGE('',*,*,#9436,.F.);
#13108=ORIENTED_EDGE('',*,*,#9437,.T.);
#13109=ORIENTED_EDGE('',*,*,#9441,.T.);
#13110=ORIENTED_EDGE('',*,*,#9442,.T.);
#13111=ORIENTED_EDGE('',*,*,#9443,.T.);
#13112=ORIENTED_EDGE('',*,*,#9444,.T.);
#13113=ORIENTED_EDGE('',*,*,#9445,.F.);
#13114=ORIENTED_EDGE('',*,*,#9446,.T.);
#13115=ORIENTED_EDGE('',*,*,#9447,.T.);
#13116=ORIENTED_EDGE('',*,*,#9448,.T.);
#13117=ORIENTED_EDGE('',*,*,#9449,.T.);
#13118=ORIENTED_EDGE('',*,*,#9447,.F.);
#13119=ORIENTED_EDGE('',*,*,#9450,.T.);
#13120=ORIENTED_EDGE('',*,*,#9451,.F.);
#13121=ORIENTED_EDGE('',*,*,#9452,.T.);
#13122=ORIENTED_EDGE('',*,*,#8302,.T.);
#13123=ORIENTED_EDGE('',*,*,#9453,.F.);
#13124=ORIENTED_EDGE('',*,*,#9446,.F.);
#13125=ORIENTED_EDGE('',*,*,#9454,.F.);
#13126=ORIENTED_EDGE('',*,*,#9455,.F.);
#13127=ORIENTED_EDGE('',*,*,#9450,.F.);
#13128=ORIENTED_EDGE('',*,*,#9451,.T.);
#13129=ORIENTED_EDGE('',*,*,#9455,.T.);
#13130=ORIENTED_EDGE('',*,*,#9456,.T.);
#13131=ORIENTED_EDGE('',*,*,#9457,.T.);
#13132=ORIENTED_EDGE('',*,*,#9458,.T.);
#13133=ORIENTED_EDGE('',*,*,#9459,.F.);
#13134=ORIENTED_EDGE('',*,*,#9460,.T.);
#13135=ORIENTED_EDGE('',*,*,#9461,.T.);
#13136=ORIENTED_EDGE('',*,*,#9462,.T.);
#13137=ORIENTED_EDGE('',*,*,#9463,.T.);
#13138=ORIENTED_EDGE('',*,*,#9461,.F.);
#13139=ORIENTED_EDGE('',*,*,#9464,.T.);
#13140=ORIENTED_EDGE('',*,*,#9465,.F.);
#13141=ORIENTED_EDGE('',*,*,#9466,.T.);
#13142=ORIENTED_EDGE('',*,*,#8304,.T.);
#13143=ORIENTED_EDGE('',*,*,#9467,.F.);
#13144=ORIENTED_EDGE('',*,*,#9460,.F.);
#13145=ORIENTED_EDGE('',*,*,#9468,.F.);
#13146=ORIENTED_EDGE('',*,*,#9469,.F.);
#13147=ORIENTED_EDGE('',*,*,#9464,.F.);
#13148=ORIENTED_EDGE('',*,*,#9470,.F.);
#13149=ORIENTED_EDGE('',*,*,#8047,.T.);
#13150=ORIENTED_EDGE('',*,*,#8052,.T.);
#13151=ORIENTED_EDGE('',*,*,#9471,.T.);
#13152=ORIENTED_EDGE('',*,*,#9472,.T.);
#13153=ORIENTED_EDGE('',*,*,#9472,.F.);
#13154=ORIENTED_EDGE('',*,*,#9473,.F.);
#13155=ORIENTED_EDGE('',*,*,#9474,.F.);
#13156=ORIENTED_EDGE('',*,*,#9475,.T.);
#13157=ORIENTED_EDGE('',*,*,#9471,.F.);
#13158=ORIENTED_EDGE('',*,*,#8051,.F.);
#13159=ORIENTED_EDGE('',*,*,#8305,.T.);
#13160=ORIENTED_EDGE('',*,*,#9466,.F.);
#13161=ORIENTED_EDGE('',*,*,#9476,.F.);
#13162=ORIENTED_EDGE('',*,*,#9473,.T.);
#13163=ORIENTED_EDGE('',*,*,#9465,.T.);
#13164=ORIENTED_EDGE('',*,*,#9469,.T.);
#13165=ORIENTED_EDGE('',*,*,#9477,.T.);
#13166=ORIENTED_EDGE('',*,*,#9474,.T.);
#13167=ORIENTED_EDGE('',*,*,#9476,.T.);
#13168=ORIENTED_EDGE('',*,*,#9360,.F.);
#13169=ORIENTED_EDGE('',*,*,#9478,.T.);
#13170=ORIENTED_EDGE('',*,*,#9364,.F.);
#13171=ORIENTED_EDGE('',*,*,#9369,.T.);
#13172=ORIENTED_EDGE('',*,*,#8289,.T.);
#13173=ORIENTED_EDGE('',*,*,#9355,.F.);
#13174=ORIENTED_EDGE('',*,*,#9374,.F.);
#13175=ORIENTED_EDGE('',*,*,#9479,.T.);
#13176=ORIENTED_EDGE('',*,*,#9378,.F.);
#13177=ORIENTED_EDGE('',*,*,#9383,.T.);
#13178=ORIENTED_EDGE('',*,*,#8291,.T.);
#13179=ORIENTED_EDGE('',*,*,#9368,.F.);
#13180=ORIENTED_EDGE('',*,*,#9388,.F.);
#13181=ORIENTED_EDGE('',*,*,#9480,.T.);
#13182=ORIENTED_EDGE('',*,*,#9392,.F.);
#13183=ORIENTED_EDGE('',*,*,#9397,.T.);
#13184=ORIENTED_EDGE('',*,*,#8293,.T.);
#13185=ORIENTED_EDGE('',*,*,#9382,.F.);
#13186=ORIENTED_EDGE('',*,*,#9402,.F.);
#13187=ORIENTED_EDGE('',*,*,#9481,.T.);
#13188=ORIENTED_EDGE('',*,*,#9406,.F.);
#13189=ORIENTED_EDGE('',*,*,#9411,.T.);
#13190=ORIENTED_EDGE('',*,*,#8295,.T.);
#13191=ORIENTED_EDGE('',*,*,#9396,.F.);
#13192=ORIENTED_EDGE('',*,*,#9416,.F.);
#13193=ORIENTED_EDGE('',*,*,#9482,.T.);
#13194=ORIENTED_EDGE('',*,*,#9420,.F.);
#13195=ORIENTED_EDGE('',*,*,#9425,.T.);
#13196=ORIENTED_EDGE('',*,*,#8297,.T.);
#13197=ORIENTED_EDGE('',*,*,#9410,.F.);
#13198=ORIENTED_EDGE('',*,*,#9430,.F.);
#13199=ORIENTED_EDGE('',*,*,#9483,.T.);
#13200=ORIENTED_EDGE('',*,*,#9434,.F.);
#13201=ORIENTED_EDGE('',*,*,#9439,.T.);
#13202=ORIENTED_EDGE('',*,*,#8299,.T.);
#13203=ORIENTED_EDGE('',*,*,#9424,.F.);
#13204=ORIENTED_EDGE('',*,*,#9444,.F.);
#13205=ORIENTED_EDGE('',*,*,#9484,.T.);
#13206=ORIENTED_EDGE('',*,*,#9448,.F.);
#13207=ORIENTED_EDGE('',*,*,#9453,.T.);
#13208=ORIENTED_EDGE('',*,*,#8301,.T.);
#13209=ORIENTED_EDGE('',*,*,#9438,.F.);
#13210=ORIENTED_EDGE('',*,*,#9458,.F.);
#13211=ORIENTED_EDGE('',*,*,#9485,.T.);
#13212=ORIENTED_EDGE('',*,*,#9462,.F.);
#13213=ORIENTED_EDGE('',*,*,#9467,.T.);
#13214=ORIENTED_EDGE('',*,*,#8303,.T.);
#13215=ORIENTED_EDGE('',*,*,#9452,.F.);
#13216=ORIENTED_EDGE('',*,*,#9457,.F.);
#13217=ORIENTED_EDGE('',*,*,#9486,.T.);
#13218=ORIENTED_EDGE('',*,*,#9463,.F.);
#13219=ORIENTED_EDGE('',*,*,#9485,.F.);
#13220=ORIENTED_EDGE('',*,*,#9443,.F.);
#13221=ORIENTED_EDGE('',*,*,#9487,.T.);
#13222=ORIENTED_EDGE('',*,*,#9449,.F.);
#13223=ORIENTED_EDGE('',*,*,#9484,.F.);
#13224=ORIENTED_EDGE('',*,*,#9429,.F.);
#13225=ORIENTED_EDGE('',*,*,#9488,.T.);
#13226=ORIENTED_EDGE('',*,*,#9435,.F.);
#13227=ORIENTED_EDGE('',*,*,#9483,.F.);
#13228=ORIENTED_EDGE('',*,*,#9415,.F.);
#13229=ORIENTED_EDGE('',*,*,#9489,.T.);
#13230=ORIENTED_EDGE('',*,*,#9421,.F.);
#13231=ORIENTED_EDGE('',*,*,#9482,.F.);
#13232=ORIENTED_EDGE('',*,*,#9401,.F.);
#13233=ORIENTED_EDGE('',*,*,#9490,.T.);
#13234=ORIENTED_EDGE('',*,*,#9407,.F.);
#13235=ORIENTED_EDGE('',*,*,#9481,.F.);
#13236=ORIENTED_EDGE('',*,*,#9387,.F.);
#13237=ORIENTED_EDGE('',*,*,#9491,.T.);
#13238=ORIENTED_EDGE('',*,*,#9393,.F.);
#13239=ORIENTED_EDGE('',*,*,#9480,.F.);
#13240=ORIENTED_EDGE('',*,*,#9373,.F.);
#13241=ORIENTED_EDGE('',*,*,#9492,.T.);
#13242=ORIENTED_EDGE('',*,*,#9379,.F.);
#13243=ORIENTED_EDGE('',*,*,#9479,.F.);
#13244=ORIENTED_EDGE('',*,*,#9359,.F.);
#13245=ORIENTED_EDGE('',*,*,#9493,.T.);
#13246=ORIENTED_EDGE('',*,*,#9365,.F.);
#13247=ORIENTED_EDGE('',*,*,#9478,.F.);
#13248=ORIENTED_EDGE('',*,*,#9494,.T.);
#13249=ORIENTED_EDGE('',*,*,#9495,.T.);
#13250=ORIENTED_EDGE('',*,*,#8426,.T.);
#13251=ORIENTED_EDGE('',*,*,#9495,.F.);
#13252=ORIENTED_EDGE('',*,*,#9496,.F.);
#13253=ORIENTED_EDGE('',*,*,#9497,.T.);
#13254=ORIENTED_EDGE('',*,*,#9494,.F.);
#13255=ORIENTED_EDGE('',*,*,#9497,.F.);
#13256=ORIENTED_EDGE('',*,*,#9498,.T.);
#13257=ORIENTED_EDGE('',*,*,#9499,.F.);
#13258=ORIENTED_EDGE('',*,*,#8129,.T.);
#13259=ORIENTED_EDGE('',*,*,#8134,.T.);
#13260=ORIENTED_EDGE('',*,*,#8127,.F.);
#13261=ORIENTED_EDGE('',*,*,#9500,.T.);
#13262=ORIENTED_EDGE('',*,*,#8138,.F.);
#13263=ORIENTED_EDGE('',*,*,#8144,.T.);
#13264=ORIENTED_EDGE('',*,*,#8280,.T.);
#13265=ORIENTED_EDGE('',*,*,#8131,.F.);
#13266=ORIENTED_EDGE('',*,*,#8149,.F.);
#13267=ORIENTED_EDGE('',*,*,#9501,.T.);
#13268=ORIENTED_EDGE('',*,*,#8153,.F.);
#13269=ORIENTED_EDGE('',*,*,#8159,.T.);
#13270=ORIENTED_EDGE('',*,*,#8281,.T.);
#13271=ORIENTED_EDGE('',*,*,#8142,.F.);
#13272=ORIENTED_EDGE('',*,*,#8164,.F.);
#13273=ORIENTED_EDGE('',*,*,#9502,.T.);
#13274=ORIENTED_EDGE('',*,*,#8168,.F.);
#13275=ORIENTED_EDGE('',*,*,#8174,.T.);
#13276=ORIENTED_EDGE('',*,*,#8282,.T.);
#13277=ORIENTED_EDGE('',*,*,#8157,.F.);
#13278=ORIENTED_EDGE('',*,*,#8179,.F.);
#13279=ORIENTED_EDGE('',*,*,#9503,.T.);
#13280=ORIENTED_EDGE('',*,*,#8183,.F.);
#13281=ORIENTED_EDGE('',*,*,#8189,.T.);
#13282=ORIENTED_EDGE('',*,*,#8283,.T.);
#13283=ORIENTED_EDGE('',*,*,#8172,.F.);
#13284=ORIENTED_EDGE('',*,*,#8194,.F.);
#13285=ORIENTED_EDGE('',*,*,#9504,.T.);
#13286=ORIENTED_EDGE('',*,*,#8198,.F.);
#13287=ORIENTED_EDGE('',*,*,#8204,.T.);
#13288=ORIENTED_EDGE('',*,*,#8284,.T.);
#13289=ORIENTED_EDGE('',*,*,#8187,.F.);
#13290=ORIENTED_EDGE('',*,*,#8209,.F.);
#13291=ORIENTED_EDGE('',*,*,#9505,.T.);
#13292=ORIENTED_EDGE('',*,*,#8213,.F.);
#13293=ORIENTED_EDGE('',*,*,#8219,.T.);
#13294=ORIENTED_EDGE('',*,*,#8285,.T.);
#13295=ORIENTED_EDGE('',*,*,#8202,.F.);
#13296=ORIENTED_EDGE('',*,*,#8224,.F.);
#13297=ORIENTED_EDGE('',*,*,#9506,.T.);
#13298=ORIENTED_EDGE('',*,*,#8228,.F.);
#13299=ORIENTED_EDGE('',*,*,#8234,.T.);
#13300=ORIENTED_EDGE('',*,*,#8286,.T.);
#13301=ORIENTED_EDGE('',*,*,#8217,.F.);
#13302=ORIENTED_EDGE('',*,*,#8239,.F.);
#13303=ORIENTED_EDGE('',*,*,#9507,.T.);
#13304=ORIENTED_EDGE('',*,*,#8243,.F.);
#13305=ORIENTED_EDGE('',*,*,#8249,.T.);
#13306=ORIENTED_EDGE('',*,*,#8287,.T.);
#13307=ORIENTED_EDGE('',*,*,#8232,.F.);
#13308=ORIENTED_EDGE('',*,*,#8253,.F.);
#13309=ORIENTED_EDGE('',*,*,#9508,.T.);
#13310=ORIENTED_EDGE('',*,*,#9352,.F.);
#13311=ORIENTED_EDGE('',*,*,#8255,.F.);
#13312=ORIENTED_EDGE('',*,*,#8238,.F.);
#13313=ORIENTED_EDGE('',*,*,#9509,.T.);
#13314=ORIENTED_EDGE('',*,*,#8244,.F.);
#13315=ORIENTED_EDGE('',*,*,#9507,.F.);
#13316=ORIENTED_EDGE('',*,*,#8223,.F.);
#13317=ORIENTED_EDGE('',*,*,#9510,.T.);
#13318=ORIENTED_EDGE('',*,*,#8229,.F.);
#13319=ORIENTED_EDGE('',*,*,#9506,.F.);
#13320=ORIENTED_EDGE('',*,*,#8208,.F.);
#13321=ORIENTED_EDGE('',*,*,#9511,.T.);
#13322=ORIENTED_EDGE('',*,*,#8214,.F.);
#13323=ORIENTED_EDGE('',*,*,#9505,.F.);
#13324=ORIENTED_EDGE('',*,*,#8193,.F.);
#13325=ORIENTED_EDGE('',*,*,#9512,.T.);
#13326=ORIENTED_EDGE('',*,*,#8199,.F.);
#13327=ORIENTED_EDGE('',*,*,#9504,.F.);
#13328=ORIENTED_EDGE('',*,*,#8178,.F.);
#13329=ORIENTED_EDGE('',*,*,#9513,.T.);
#13330=ORIENTED_EDGE('',*,*,#8184,.F.);
#13331=ORIENTED_EDGE('',*,*,#9503,.F.);
#13332=ORIENTED_EDGE('',*,*,#8163,.F.);
#13333=ORIENTED_EDGE('',*,*,#9514,.T.);
#13334=ORIENTED_EDGE('',*,*,#8169,.F.);
#13335=ORIENTED_EDGE('',*,*,#9502,.F.);
#13336=ORIENTED_EDGE('',*,*,#8148,.F.);
#13337=ORIENTED_EDGE('',*,*,#9515,.T.);
#13338=ORIENTED_EDGE('',*,*,#8154,.F.);
#13339=ORIENTED_EDGE('',*,*,#9501,.F.);
#13340=ORIENTED_EDGE('',*,*,#8126,.F.);
#13341=ORIENTED_EDGE('',*,*,#9516,.T.);
#13342=ORIENTED_EDGE('',*,*,#8139,.F.);
#13343=ORIENTED_EDGE('',*,*,#9500,.F.);
#13344=ORIENTED_EDGE('',*,*,#9517,.T.);
#13345=ORIENTED_EDGE('',*,*,#9518,.T.);
#13346=ORIENTED_EDGE('',*,*,#9519,.T.);
#13347=ORIENTED_EDGE('',*,*,#8120,.F.);
#13348=ORIENTED_EDGE('',*,*,#8133,.F.);
#13349=ORIENTED_EDGE('',*,*,#8279,.F.);
#13350=ORIENTED_EDGE('',*,*,#8121,.F.);
#13351=ORIENTED_EDGE('',*,*,#9519,.F.);
#13352=ORIENTED_EDGE('',*,*,#9520,.T.);
#13353=ORIENTED_EDGE('',*,*,#9498,.F.);
#13354=ORIENTED_EDGE('',*,*,#8429,.T.);
#13355=ORIENTED_EDGE('',*,*,#9521,.F.);
#13356=ORIENTED_EDGE('',*,*,#9522,.T.);
#13357=ORIENTED_EDGE('',*,*,#9523,.T.);
#13358=ORIENTED_EDGE('',*,*,#9524,.T.);
#13359=ORIENTED_EDGE('',*,*,#9525,.T.);
#13360=ORIENTED_EDGE('',*,*,#9526,.T.);
#13361=ORIENTED_EDGE('',*,*,#8268,.T.);
#13362=ORIENTED_EDGE('',*,*,#8430,.T.);
#13363=ORIENTED_EDGE('',*,*,#9523,.F.);
#13364=ORIENTED_EDGE('',*,*,#9527,.T.);
#13365=ORIENTED_EDGE('',*,*,#9528,.T.);
#13366=ORIENTED_EDGE('',*,*,#9529,.T.);
#13367=ORIENTED_EDGE('',*,*,#9525,.F.);
#13368=ORIENTED_EDGE('',*,*,#9526,.F.);
#13369=ORIENTED_EDGE('',*,*,#9529,.F.);
#13370=ORIENTED_EDGE('',*,*,#9530,.T.);
#13371=ORIENTED_EDGE('',*,*,#9531,.F.);
#13372=ORIENTED_EDGE('',*,*,#9532,.F.);
#13373=ORIENTED_EDGE('',*,*,#8269,.F.);
#13374=ORIENTED_EDGE('',*,*,#9533,.T.);
#13375=ORIENTED_EDGE('',*,*,#9534,.F.);
#13376=ORIENTED_EDGE('',*,*,#9535,.T.);
#13377=ORIENTED_EDGE('',*,*,#9536,.T.);
#13378=ORIENTED_EDGE('',*,*,#9537,.T.);
#13379=ORIENTED_EDGE('',*,*,#9538,.T.);
#13380=ORIENTED_EDGE('',*,*,#8116,.T.);
#13381=ORIENTED_EDGE('',*,*,#8278,.T.);
#13382=ORIENTED_EDGE('',*,*,#9539,.T.);
#13383=ORIENTED_EDGE('',*,*,#9536,.F.);
#13384=ORIENTED_EDGE('',*,*,#9540,.T.);
#13385=ORIENTED_EDGE('',*,*,#9541,.T.);
#13386=ORIENTED_EDGE('',*,*,#8117,.T.);
#13387=ORIENTED_EDGE('',*,*,#9538,.F.);
#13388=ORIENTED_EDGE('',*,*,#9533,.F.);
#13389=ORIENTED_EDGE('',*,*,#9539,.F.);
#13390=ORIENTED_EDGE('',*,*,#8277,.F.);
#13391=ORIENTED_EDGE('',*,*,#9542,.F.);
#13392=ORIENTED_EDGE('',*,*,#9543,.F.);
#13393=ORIENTED_EDGE('',*,*,#9544,.T.);
#13394=ORIENTED_EDGE('',*,*,#9531,.T.);
#13395=ORIENTED_EDGE('',*,*,#9545,.F.);
#13396=ORIENTED_EDGE('',*,*,#9546,.T.);
#13397=ORIENTED_EDGE('',*,*,#9547,.T.);
#13398=ORIENTED_EDGE('',*,*,#9548,.T.);
#13399=ORIENTED_EDGE('',*,*,#9549,.T.);
#13400=ORIENTED_EDGE('',*,*,#9550,.T.);
#13401=ORIENTED_EDGE('',*,*,#8270,.T.);
#13402=ORIENTED_EDGE('',*,*,#9532,.T.);
#13403=ORIENTED_EDGE('',*,*,#9547,.F.);
#13404=ORIENTED_EDGE('',*,*,#9551,.T.);
#13405=ORIENTED_EDGE('',*,*,#9552,.T.);
#13406=ORIENTED_EDGE('',*,*,#9553,.T.);
#13407=ORIENTED_EDGE('',*,*,#9549,.F.);
#13408=ORIENTED_EDGE('',*,*,#9550,.F.);
#13409=ORIENTED_EDGE('',*,*,#9553,.F.);
#13410=ORIENTED_EDGE('',*,*,#9554,.T.);
#13411=ORIENTED_EDGE('',*,*,#9555,.F.);
#13412=ORIENTED_EDGE('',*,*,#9556,.F.);
#13413=ORIENTED_EDGE('',*,*,#8271,.F.);
#13414=ORIENTED_EDGE('',*,*,#9557,.T.);
#13415=ORIENTED_EDGE('',*,*,#9558,.F.);
#13416=ORIENTED_EDGE('',*,*,#9559,.T.);
#13417=ORIENTED_EDGE('',*,*,#9560,.T.);
#13418=ORIENTED_EDGE('',*,*,#9561,.T.);
#13419=ORIENTED_EDGE('',*,*,#9562,.T.);
#13420=ORIENTED_EDGE('',*,*,#9542,.T.);
#13421=ORIENTED_EDGE('',*,*,#8276,.T.);
#13422=ORIENTED_EDGE('',*,*,#9563,.T.);
#13423=ORIENTED_EDGE('',*,*,#9560,.F.);
#13424=ORIENTED_EDGE('',*,*,#9564,.T.);
#13425=ORIENTED_EDGE('',*,*,#9565,.T.);
#13426=ORIENTED_EDGE('',*,*,#9543,.T.);
#13427=ORIENTED_EDGE('',*,*,#9562,.F.);
#13428=ORIENTED_EDGE('',*,*,#9557,.F.);
#13429=ORIENTED_EDGE('',*,*,#9563,.F.);
#13430=ORIENTED_EDGE('',*,*,#8275,.F.);
#13431=ORIENTED_EDGE('',*,*,#9566,.F.);
#13432=ORIENTED_EDGE('',*,*,#9567,.F.);
#13433=ORIENTED_EDGE('',*,*,#9568,.T.);
#13434=ORIENTED_EDGE('',*,*,#9555,.T.);
#13435=ORIENTED_EDGE('',*,*,#9569,.F.);
#13436=ORIENTED_EDGE('',*,*,#9570,.T.);
#13437=ORIENTED_EDGE('',*,*,#9571,.T.);
#13438=ORIENTED_EDGE('',*,*,#9572,.T.);
#13439=ORIENTED_EDGE('',*,*,#9573,.T.);
#13440=ORIENTED_EDGE('',*,*,#9574,.T.);
#13441=ORIENTED_EDGE('',*,*,#8272,.T.);
#13442=ORIENTED_EDGE('',*,*,#9556,.T.);
#13443=ORIENTED_EDGE('',*,*,#9571,.F.);
#13444=ORIENTED_EDGE('',*,*,#9575,.T.);
#13445=ORIENTED_EDGE('',*,*,#9576,.T.);
#13446=ORIENTED_EDGE('',*,*,#9577,.T.);
#13447=ORIENTED_EDGE('',*,*,#9573,.F.);
#13448=ORIENTED_EDGE('',*,*,#9574,.F.);
#13449=ORIENTED_EDGE('',*,*,#9577,.F.);
#13450=ORIENTED_EDGE('',*,*,#9578,.T.);
#13451=ORIENTED_EDGE('',*,*,#9579,.F.);
#13452=ORIENTED_EDGE('',*,*,#9580,.F.);
#13453=ORIENTED_EDGE('',*,*,#8273,.F.);
#13454=ORIENTED_EDGE('',*,*,#9579,.T.);
#13455=ORIENTED_EDGE('',*,*,#9581,.F.);
#13456=ORIENTED_EDGE('',*,*,#9582,.T.);
#13457=ORIENTED_EDGE('',*,*,#9583,.T.);
#13458=ORIENTED_EDGE('',*,*,#9584,.T.);
#13459=ORIENTED_EDGE('',*,*,#9585,.T.);
#13460=ORIENTED_EDGE('',*,*,#9566,.T.);
#13461=ORIENTED_EDGE('',*,*,#8274,.T.);
#13462=ORIENTED_EDGE('',*,*,#9580,.T.);
#13463=ORIENTED_EDGE('',*,*,#9583,.F.);
#13464=ORIENTED_EDGE('',*,*,#9586,.T.);
#13465=ORIENTED_EDGE('',*,*,#9587,.T.);
#13466=ORIENTED_EDGE('',*,*,#9567,.T.);
#13467=ORIENTED_EDGE('',*,*,#9585,.F.);
#13468=ORIENTED_EDGE('',*,*,#9588,.T.);
#13469=ORIENTED_EDGE('',*,*,#9589,.T.);
#13470=ORIENTED_EDGE('',*,*,#9590,.T.);
#13471=ORIENTED_EDGE('',*,*,#9589,.F.);
#13472=ORIENTED_EDGE('',*,*,#9590,.F.);
#13473=ORIENTED_EDGE('',*,*,#9591,.F.);
#13474=ORIENTED_EDGE('',*,*,#9588,.F.);
#13475=ORIENTED_EDGE('',*,*,#9592,.T.);
#13476=ORIENTED_EDGE('',*,*,#9593,.T.);
#13477=ORIENTED_EDGE('',*,*,#9594,.T.);
#13478=ORIENTED_EDGE('',*,*,#9595,.T.);
#13479=ORIENTED_EDGE('',*,*,#9596,.T.);
#13480=ORIENTED_EDGE('',*,*,#9597,.T.);
#13481=ORIENTED_EDGE('',*,*,#9598,.T.);
#13482=ORIENTED_EDGE('',*,*,#9599,.T.);
#13483=ORIENTED_EDGE('',*,*,#9600,.T.);
#13484=ORIENTED_EDGE('',*,*,#9601,.T.);
#13485=ORIENTED_EDGE('',*,*,#9602,.T.);
#13486=ORIENTED_EDGE('',*,*,#9603,.T.);
#13487=ORIENTED_EDGE('',*,*,#9604,.T.);
#13488=ORIENTED_EDGE('',*,*,#9605,.T.);
#13489=ORIENTED_EDGE('',*,*,#9606,.T.);
#13490=ORIENTED_EDGE('',*,*,#9607,.T.);
#13491=ORIENTED_EDGE('',*,*,#8060,.T.);
#13492=ORIENTED_EDGE('',*,*,#9608,.T.);
#13493=ORIENTED_EDGE('',*,*,#8477,.T.);
#13494=ORIENTED_EDGE('',*,*,#9609,.T.);
#13495=ORIENTED_EDGE('',*,*,#8568,.T.);
#13496=ORIENTED_EDGE('',*,*,#9610,.T.);
#13497=ORIENTED_EDGE('',*,*,#8569,.T.);
#13498=ORIENTED_EDGE('',*,*,#9611,.T.);
#13499=ORIENTED_EDGE('',*,*,#8570,.T.);
#13500=ORIENTED_EDGE('',*,*,#9612,.T.);
#13501=ORIENTED_EDGE('',*,*,#8558,.T.);
#13502=ORIENTED_EDGE('',*,*,#9613,.T.);
#13503=ORIENTED_EDGE('',*,*,#8544,.T.);
#13504=ORIENTED_EDGE('',*,*,#9614,.T.);
#13505=ORIENTED_EDGE('',*,*,#8530,.T.);
#13506=ORIENTED_EDGE('',*,*,#9615,.T.);
#13507=ORIENTED_EDGE('',*,*,#8516,.T.);
#13508=ORIENTED_EDGE('',*,*,#9616,.T.);
#13509=ORIENTED_EDGE('',*,*,#8502,.T.);
#13510=ORIENTED_EDGE('',*,*,#9617,.T.);
#13511=ORIENTED_EDGE('',*,*,#8488,.T.);
#13512=ORIENTED_EDGE('',*,*,#9618,.T.);
#13513=ORIENTED_EDGE('',*,*,#8644,.T.);
#13514=ORIENTED_EDGE('',*,*,#9619,.T.);
#13515=ORIENTED_EDGE('',*,*,#8722,.T.);
#13516=ORIENTED_EDGE('',*,*,#9620,.T.);
#13517=ORIENTED_EDGE('',*,*,#8723,.T.);
#13518=ORIENTED_EDGE('',*,*,#9621,.T.);
#13519=ORIENTED_EDGE('',*,*,#8724,.T.);
#13520=ORIENTED_EDGE('',*,*,#9622,.T.);
#13521=ORIENTED_EDGE('',*,*,#8725,.T.);
#13522=ORIENTED_EDGE('',*,*,#9623,.T.);
#13523=ORIENTED_EDGE('',*,*,#8712,.T.);
#13524=ORIENTED_EDGE('',*,*,#9624,.T.);
#13525=ORIENTED_EDGE('',*,*,#8698,.T.);
#13526=ORIENTED_EDGE('',*,*,#9625,.T.);
#13527=ORIENTED_EDGE('',*,*,#8684,.T.);
#13528=ORIENTED_EDGE('',*,*,#9626,.T.);
#13529=ORIENTED_EDGE('',*,*,#8670,.T.);
#13530=ORIENTED_EDGE('',*,*,#9627,.T.);
#13531=ORIENTED_EDGE('',*,*,#8656,.T.);
#13532=ORIENTED_EDGE('',*,*,#9628,.T.);
#13533=ORIENTED_EDGE('',*,*,#8810,.T.);
#13534=ORIENTED_EDGE('',*,*,#9629,.T.);
#13535=ORIENTED_EDGE('',*,*,#8876,.T.);
#13536=ORIENTED_EDGE('',*,*,#9630,.T.);
#13537=ORIENTED_EDGE('',*,*,#8877,.T.);
#13538=ORIENTED_EDGE('',*,*,#9631,.T.);
#13539=ORIENTED_EDGE('',*,*,#8878,.T.);
#13540=ORIENTED_EDGE('',*,*,#9632,.T.);
#13541=ORIENTED_EDGE('',*,*,#8879,.T.);
#13542=ORIENTED_EDGE('',*,*,#9633,.T.);
#13543=ORIENTED_EDGE('',*,*,#8880,.T.);
#13544=ORIENTED_EDGE('',*,*,#9634,.T.);
#13545=ORIENTED_EDGE('',*,*,#8864,.T.);
#13546=ORIENTED_EDGE('',*,*,#9635,.T.);
#13547=ORIENTED_EDGE('',*,*,#8850,.T.);
#13548=ORIENTED_EDGE('',*,*,#9636,.T.);
#13549=ORIENTED_EDGE('',*,*,#8836,.T.);
#13550=ORIENTED_EDGE('',*,*,#9637,.T.);
#13551=ORIENTED_EDGE('',*,*,#8822,.T.);
#13552=ORIENTED_EDGE('',*,*,#9638,.T.);
#13553=ORIENTED_EDGE('',*,*,#8978,.T.);
#13554=ORIENTED_EDGE('',*,*,#9639,.T.);
#13555=ORIENTED_EDGE('',*,*,#9030,.T.);
#13556=ORIENTED_EDGE('',*,*,#9640,.T.);
#13557=ORIENTED_EDGE('',*,*,#9031,.T.);
#13558=ORIENTED_EDGE('',*,*,#9641,.T.);
#13559=ORIENTED_EDGE('',*,*,#9032,.T.);
#13560=ORIENTED_EDGE('',*,*,#9642,.T.);
#13561=ORIENTED_EDGE('',*,*,#9033,.T.);
#13562=ORIENTED_EDGE('',*,*,#9643,.T.);
#13563=ORIENTED_EDGE('',*,*,#9034,.T.);
#13564=ORIENTED_EDGE('',*,*,#9644,.T.);
#13565=ORIENTED_EDGE('',*,*,#9035,.T.);
#13566=ORIENTED_EDGE('',*,*,#9645,.T.);
#13567=ORIENTED_EDGE('',*,*,#9018,.T.);
#13568=ORIENTED_EDGE('',*,*,#9646,.T.);
#13569=ORIENTED_EDGE('',*,*,#9004,.T.);
#13570=ORIENTED_EDGE('',*,*,#9647,.T.);
#13571=ORIENTED_EDGE('',*,*,#8990,.T.);
#13572=ORIENTED_EDGE('',*,*,#9648,.T.);
#13573=ORIENTED_EDGE('',*,*,#9144,.T.);
#13574=ORIENTED_EDGE('',*,*,#9649,.T.);
#13575=ORIENTED_EDGE('',*,*,#9184,.T.);
#13576=ORIENTED_EDGE('',*,*,#9650,.T.);
#13577=ORIENTED_EDGE('',*,*,#9185,.T.);
#13578=ORIENTED_EDGE('',*,*,#9651,.T.);
#13579=ORIENTED_EDGE('',*,*,#9186,.T.);
#13580=ORIENTED_EDGE('',*,*,#9652,.T.);
#13581=ORIENTED_EDGE('',*,*,#9187,.T.);
#13582=ORIENTED_EDGE('',*,*,#9653,.T.);
#13583=ORIENTED_EDGE('',*,*,#9188,.T.);
#13584=ORIENTED_EDGE('',*,*,#9654,.T.);
#13585=ORIENTED_EDGE('',*,*,#9189,.T.);
#13586=ORIENTED_EDGE('',*,*,#9655,.T.);
#13587=ORIENTED_EDGE('',*,*,#9190,.T.);
#13588=ORIENTED_EDGE('',*,*,#9656,.T.);
#13589=ORIENTED_EDGE('',*,*,#9170,.T.);
#13590=ORIENTED_EDGE('',*,*,#9657,.T.);
#13591=ORIENTED_EDGE('',*,*,#9156,.T.);
#13592=ORIENTED_EDGE('',*,*,#9658,.T.);
#13593=ORIENTED_EDGE('',*,*,#9311,.T.);
#13594=ORIENTED_EDGE('',*,*,#9659,.T.);
#13595=ORIENTED_EDGE('',*,*,#9338,.T.);
#13596=ORIENTED_EDGE('',*,*,#9660,.T.);
#13597=ORIENTED_EDGE('',*,*,#9339,.T.);
#13598=ORIENTED_EDGE('',*,*,#9661,.T.);
#13599=ORIENTED_EDGE('',*,*,#9340,.T.);
#13600=ORIENTED_EDGE('',*,*,#9662,.T.);
#13601=ORIENTED_EDGE('',*,*,#9341,.T.);
#13602=ORIENTED_EDGE('',*,*,#9663,.T.);
#13603=ORIENTED_EDGE('',*,*,#9342,.T.);
#13604=ORIENTED_EDGE('',*,*,#9664,.T.);
#13605=ORIENTED_EDGE('',*,*,#9343,.T.);
#13606=ORIENTED_EDGE('',*,*,#9665,.T.);
#13607=ORIENTED_EDGE('',*,*,#9344,.T.);
#13608=ORIENTED_EDGE('',*,*,#9666,.T.);
#13609=ORIENTED_EDGE('',*,*,#9345,.T.);
#13610=ORIENTED_EDGE('',*,*,#9667,.T.);
#13611=ORIENTED_EDGE('',*,*,#9323,.T.);
#13612=ORIENTED_EDGE('',*,*,#9668,.T.);
#13613=ORIENTED_EDGE('',*,*,#8048,.T.);
#13614=ORIENTED_EDGE('',*,*,#9669,.T.);
#13615=ORIENTED_EDGE('',*,*,#9468,.T.);
#13616=ORIENTED_EDGE('',*,*,#9670,.T.);
#13617=ORIENTED_EDGE('',*,*,#9454,.T.);
#13618=ORIENTED_EDGE('',*,*,#9671,.T.);
#13619=ORIENTED_EDGE('',*,*,#9440,.T.);
#13620=ORIENTED_EDGE('',*,*,#9672,.T.);
#13621=ORIENTED_EDGE('',*,*,#9426,.T.);
#13622=ORIENTED_EDGE('',*,*,#9673,.T.);
#13623=ORIENTED_EDGE('',*,*,#9412,.T.);
#13624=ORIENTED_EDGE('',*,*,#9674,.T.);
#13625=ORIENTED_EDGE('',*,*,#9398,.T.);
#13626=ORIENTED_EDGE('',*,*,#9675,.T.);
#13627=ORIENTED_EDGE('',*,*,#9384,.T.);
#13628=ORIENTED_EDGE('',*,*,#9676,.T.);
#13629=ORIENTED_EDGE('',*,*,#9370,.T.);
#13630=ORIENTED_EDGE('',*,*,#9677,.T.);
#13631=ORIENTED_EDGE('',*,*,#9356,.T.);
#13632=ORIENTED_EDGE('',*,*,#9678,.T.);
#13633=ORIENTED_EDGE('',*,*,#8250,.T.);
#13634=ORIENTED_EDGE('',*,*,#9679,.T.);
#13635=ORIENTED_EDGE('',*,*,#8235,.T.);
#13636=ORIENTED_EDGE('',*,*,#9680,.T.);
#13637=ORIENTED_EDGE('',*,*,#8220,.T.);
#13638=ORIENTED_EDGE('',*,*,#9681,.T.);
#13639=ORIENTED_EDGE('',*,*,#8205,.T.);
#13640=ORIENTED_EDGE('',*,*,#9682,.T.);
#13641=ORIENTED_EDGE('',*,*,#8190,.T.);
#13642=ORIENTED_EDGE('',*,*,#9683,.T.);
#13643=ORIENTED_EDGE('',*,*,#8175,.T.);
#13644=ORIENTED_EDGE('',*,*,#9684,.T.);
#13645=ORIENTED_EDGE('',*,*,#8160,.T.);
#13646=ORIENTED_EDGE('',*,*,#9685,.T.);
#13647=ORIENTED_EDGE('',*,*,#8145,.T.);
#13648=ORIENTED_EDGE('',*,*,#9686,.T.);
#13649=ORIENTED_EDGE('',*,*,#8130,.T.);
#13650=ORIENTED_EDGE('',*,*,#9687,.T.);
#13651=ORIENTED_EDGE('',*,*,#9688,.T.);
#13652=ORIENTED_EDGE('',*,*,#9689,.T.);
#13653=ORIENTED_EDGE('',*,*,#9690,.T.);
#13654=ORIENTED_EDGE('',*,*,#9691,.T.);
#13655=ORIENTED_EDGE('',*,*,#9692,.T.);
#13656=ORIENTED_EDGE('',*,*,#9693,.T.);
#13657=ORIENTED_EDGE('',*,*,#9592,.F.);
#13658=ORIENTED_EDGE('',*,*,#9694,.T.);
#13659=ORIENTED_EDGE('',*,*,#9695,.T.);
#13660=ORIENTED_EDGE('',*,*,#9696,.T.);
#13661=ORIENTED_EDGE('',*,*,#9695,.F.);
#13662=ORIENTED_EDGE('',*,*,#9697,.T.);
#13663=ORIENTED_EDGE('',*,*,#9698,.F.);
#13664=ORIENTED_EDGE('',*,*,#9699,.F.);
#13665=ORIENTED_EDGE('',*,*,#9700,.T.);
#13666=ORIENTED_EDGE('',*,*,#9701,.F.);
#13667=ORIENTED_EDGE('',*,*,#9702,.F.);
#13668=ORIENTED_EDGE('',*,*,#9694,.F.);
#13669=ORIENTED_EDGE('',*,*,#9696,.F.);
#13670=ORIENTED_EDGE('',*,*,#9703,.T.);
#13671=ORIENTED_EDGE('',*,*,#9704,.F.);
#13672=ORIENTED_EDGE('',*,*,#9703,.F.);
#13673=ORIENTED_EDGE('',*,*,#9698,.T.);
#13674=ORIENTED_EDGE('',*,*,#9705,.T.);
#13675=ORIENTED_EDGE('',*,*,#9706,.T.);
#13676=ORIENTED_EDGE('',*,*,#9705,.F.);
#13677=ORIENTED_EDGE('',*,*,#9706,.F.);
#13678=ORIENTED_EDGE('',*,*,#9707,.T.);
#13679=ORIENTED_EDGE('',*,*,#9708,.F.);
#13680=ORIENTED_EDGE('',*,*,#9707,.F.);
#13681=ORIENTED_EDGE('',*,*,#9702,.T.);
#13682=ORIENTED_EDGE('',*,*,#9709,.T.);
#13683=ORIENTED_EDGE('',*,*,#9710,.T.);
#13684=ORIENTED_EDGE('',*,*,#9709,.F.);
#13685=ORIENTED_EDGE('',*,*,#9710,.F.);
#13686=ORIENTED_EDGE('',*,*,#9711,.T.);
#13687=ORIENTED_EDGE('',*,*,#9712,.F.);
#13688=ORIENTED_EDGE('',*,*,#9711,.F.);
#13689=ORIENTED_EDGE('',*,*,#9699,.T.);
#13690=ORIENTED_EDGE('',*,*,#9713,.T.);
#13691=ORIENTED_EDGE('',*,*,#9714,.T.);
#13692=ORIENTED_EDGE('',*,*,#9713,.F.);
#13693=ORIENTED_EDGE('',*,*,#9714,.F.);
#13694=ORIENTED_EDGE('',*,*,#9715,.T.);
#13695=ORIENTED_EDGE('',*,*,#9716,.F.);
#13696=ORIENTED_EDGE('',*,*,#9715,.F.);
#13697=ORIENTED_EDGE('',*,*,#9701,.T.);
#13698=ORIENTED_EDGE('',*,*,#9717,.T.);
#13699=ORIENTED_EDGE('',*,*,#9718,.T.);
#13700=ORIENTED_EDGE('',*,*,#9717,.F.);
#13701=ORIENTED_EDGE('',*,*,#9718,.F.);
#13702=ORIENTED_EDGE('',*,*,#9719,.T.);
#13703=ORIENTED_EDGE('',*,*,#9720,.F.);
#13704=ORIENTED_EDGE('',*,*,#9719,.F.);
#13705=ORIENTED_EDGE('',*,*,#9591,.T.);
#13706=ORIENTED_EDGE('',*,*,#9721,.T.);
#13707=ORIENTED_EDGE('',*,*,#9722,.T.);
#13708=ORIENTED_EDGE('',*,*,#9721,.F.);
#13709=ORIENTED_EDGE('',*,*,#9722,.F.);
#13710=ORIENTED_EDGE('',*,*,#9723,.T.);
#13711=ORIENTED_EDGE('',*,*,#9697,.F.);
#13712=ORIENTED_EDGE('',*,*,#9723,.F.);
#13713=ORIENTED_EDGE('',*,*,#9582,.F.);
#13714=ORIENTED_EDGE('',*,*,#9594,.F.);
#13715=ORIENTED_EDGE('',*,*,#9586,.F.);
#13716=ORIENTED_EDGE('',*,*,#9584,.F.);
#13717=ORIENTED_EDGE('',*,*,#9570,.F.);
#13718=ORIENTED_EDGE('',*,*,#9596,.F.);
#13719=ORIENTED_EDGE('',*,*,#9575,.F.);
#13720=ORIENTED_EDGE('',*,*,#9572,.F.);
#13721=ORIENTED_EDGE('',*,*,#9559,.F.);
#13722=ORIENTED_EDGE('',*,*,#9692,.F.);
#13723=ORIENTED_EDGE('',*,*,#9564,.F.);
#13724=ORIENTED_EDGE('',*,*,#9561,.F.);
#13725=ORIENTED_EDGE('',*,*,#9546,.F.);
#13726=ORIENTED_EDGE('',*,*,#9598,.F.);
#13727=ORIENTED_EDGE('',*,*,#9551,.F.);
#13728=ORIENTED_EDGE('',*,*,#9548,.F.);
#13729=ORIENTED_EDGE('',*,*,#9535,.F.);
#13730=ORIENTED_EDGE('',*,*,#9690,.F.);
#13731=ORIENTED_EDGE('',*,*,#9540,.F.);
#13732=ORIENTED_EDGE('',*,*,#9537,.F.);
#13733=ORIENTED_EDGE('',*,*,#9522,.F.);
#13734=ORIENTED_EDGE('',*,*,#9600,.F.);
#13735=ORIENTED_EDGE('',*,*,#9527,.F.);
#13736=ORIENTED_EDGE('',*,*,#9524,.F.);
#13737=ORIENTED_EDGE('',*,*,#8111,.F.);
#13738=ORIENTED_EDGE('',*,*,#9688,.F.);
#13739=ORIENTED_EDGE('',*,*,#9517,.F.);
#13740=ORIENTED_EDGE('',*,*,#8119,.F.);
#13741=ORIENTED_EDGE('',*,*,#8108,.F.);
#13742=ORIENTED_EDGE('',*,*,#9602,.F.);
#13743=ORIENTED_EDGE('',*,*,#8431,.F.);
#13744=ORIENTED_EDGE('',*,*,#8263,.F.);
#13745=ORIENTED_EDGE('',*,*,#8093,.F.);
#13746=ORIENTED_EDGE('',*,*,#8262,.F.);
#13747=ORIENTED_EDGE('',*,*,#8105,.F.);
#13748=ORIENTED_EDGE('',*,*,#9604,.F.);
#13749=ORIENTED_EDGE('',*,*,#8072,.F.);
#13750=ORIENTED_EDGE('',*,*,#8260,.F.);
#13751=ORIENTED_EDGE('',*,*,#8084,.F.);
#13752=ORIENTED_EDGE('',*,*,#9606,.F.);
#13753=ORIENTED_EDGE('',*,*,#9644,.F.);
#13754=ORIENTED_EDGE('',*,*,#8901,.T.);
#13755=ORIENTED_EDGE('',*,*,#8899,.F.);
#13756=ORIENTED_EDGE('',*,*,#8892,.F.);
#13757=ORIENTED_EDGE('',*,*,#9643,.F.);
#13758=ORIENTED_EDGE('',*,*,#8916,.T.);
#13759=ORIENTED_EDGE('',*,*,#8914,.F.);
#13760=ORIENTED_EDGE('',*,*,#8908,.F.);
#13761=ORIENTED_EDGE('',*,*,#9642,.F.);
#13762=ORIENTED_EDGE('',*,*,#8930,.T.);
#13763=ORIENTED_EDGE('',*,*,#8928,.F.);
#13764=ORIENTED_EDGE('',*,*,#8921,.F.);
#13765=ORIENTED_EDGE('',*,*,#9641,.F.);
#13766=ORIENTED_EDGE('',*,*,#8944,.T.);
#13767=ORIENTED_EDGE('',*,*,#8942,.F.);
#13768=ORIENTED_EDGE('',*,*,#8935,.F.);
#13769=ORIENTED_EDGE('',*,*,#9640,.F.);
#13770=ORIENTED_EDGE('',*,*,#8958,.T.);
#13771=ORIENTED_EDGE('',*,*,#8956,.F.);
#13772=ORIENTED_EDGE('',*,*,#8949,.F.);
#13773=ORIENTED_EDGE('',*,*,#9639,.F.);
#13774=ORIENTED_EDGE('',*,*,#8981,.T.);
#13775=ORIENTED_EDGE('',*,*,#8970,.F.);
#13776=ORIENTED_EDGE('',*,*,#8963,.F.);
#13777=ORIENTED_EDGE('',*,*,#8817,.F.);
#13778=ORIENTED_EDGE('',*,*,#8821,.T.);
#13779=ORIENTED_EDGE('',*,*,#8366,.F.);
#13780=ORIENTED_EDGE('',*,*,#8979,.T.);
#13781=ORIENTED_EDGE('',*,*,#8975,.F.);
#13782=ORIENTED_EDGE('',*,*,#9724,.T.);
#13783=ORIENTED_EDGE('',*,*,#9638,.F.);
#13784=ORIENTED_EDGE('',*,*,#8814,.T.);
#13785=ORIENTED_EDGE('',*,*,#9724,.F.);
#13786=ORIENTED_EDGE('',*,*,#8974,.F.);
#13787=ORIENTED_EDGE('',*,*,#9637,.F.);
#13788=ORIENTED_EDGE('',*,*,#8827,.T.);
#13789=ORIENTED_EDGE('',*,*,#8889,.F.);
#13790=ORIENTED_EDGE('',*,*,#8824,.F.);
#13791=ORIENTED_EDGE('',*,*,#9636,.F.);
#13792=ORIENTED_EDGE('',*,*,#8841,.T.);
#13793=ORIENTED_EDGE('',*,*,#8888,.F.);
#13794=ORIENTED_EDGE('',*,*,#8838,.F.);
#13795=ORIENTED_EDGE('',*,*,#9635,.F.);
#13796=ORIENTED_EDGE('',*,*,#8855,.T.);
#13797=ORIENTED_EDGE('',*,*,#8887,.F.);
#13798=ORIENTED_EDGE('',*,*,#8852,.F.);
#13799=ORIENTED_EDGE('',*,*,#9634,.F.);
#13800=ORIENTED_EDGE('',*,*,#8867,.T.);
#13801=ORIENTED_EDGE('',*,*,#8886,.F.);
#13802=ORIENTED_EDGE('',*,*,#8881,.F.);
#13803=ORIENTED_EDGE('',*,*,#9633,.F.);
#13804=ORIENTED_EDGE('',*,*,#8748,.T.);
#13805=ORIENTED_EDGE('',*,*,#8746,.F.);
#13806=ORIENTED_EDGE('',*,*,#8739,.F.);
#13807=ORIENTED_EDGE('',*,*,#9632,.F.);
#13808=ORIENTED_EDGE('',*,*,#8762,.T.);
#13809=ORIENTED_EDGE('',*,*,#8760,.F.);
#13810=ORIENTED_EDGE('',*,*,#8753,.F.);
#13811=ORIENTED_EDGE('',*,*,#9631,.F.);
#13812=ORIENTED_EDGE('',*,*,#8776,.T.);
#13813=ORIENTED_EDGE('',*,*,#8774,.F.);
#13814=ORIENTED_EDGE('',*,*,#8767,.F.);
#13815=ORIENTED_EDGE('',*,*,#9630,.F.);
#13816=ORIENTED_EDGE('',*,*,#8790,.T.);
#13817=ORIENTED_EDGE('',*,*,#8788,.F.);
#13818=ORIENTED_EDGE('',*,*,#8781,.F.);
#13819=ORIENTED_EDGE('',*,*,#9629,.F.);
#13820=ORIENTED_EDGE('',*,*,#8813,.T.);
#13821=ORIENTED_EDGE('',*,*,#8802,.F.);
#13822=ORIENTED_EDGE('',*,*,#8795,.F.);
#13823=ORIENTED_EDGE('',*,*,#8651,.F.);
#13824=ORIENTED_EDGE('',*,*,#8655,.T.);
#13825=ORIENTED_EDGE('',*,*,#8386,.F.);
#13826=ORIENTED_EDGE('',*,*,#8811,.T.);
#13827=ORIENTED_EDGE('',*,*,#8807,.F.);
#13828=ORIENTED_EDGE('',*,*,#9725,.T.);
#13829=ORIENTED_EDGE('',*,*,#9628,.F.);
#13830=ORIENTED_EDGE('',*,*,#8648,.T.);
#13831=ORIENTED_EDGE('',*,*,#9725,.F.);
#13832=ORIENTED_EDGE('',*,*,#8806,.F.);
#13833=ORIENTED_EDGE('',*,*,#9627,.F.);
#13834=ORIENTED_EDGE('',*,*,#8661,.T.);
#13835=ORIENTED_EDGE('',*,*,#8736,.F.);
#13836=ORIENTED_EDGE('',*,*,#8658,.F.);
#13837=ORIENTED_EDGE('',*,*,#9626,.F.);
#13838=ORIENTED_EDGE('',*,*,#8675,.T.);
#13839=ORIENTED_EDGE('',*,*,#8735,.F.);
#13840=ORIENTED_EDGE('',*,*,#8672,.F.);
#13841=ORIENTED_EDGE('',*,*,#9625,.F.);
#13842=ORIENTED_EDGE('',*,*,#8689,.T.);
#13843=ORIENTED_EDGE('',*,*,#8734,.F.);
#13844=ORIENTED_EDGE('',*,*,#8686,.F.);
#13845=ORIENTED_EDGE('',*,*,#9624,.F.);
#13846=ORIENTED_EDGE('',*,*,#8703,.T.);
#13847=ORIENTED_EDGE('',*,*,#8733,.F.);
#13848=ORIENTED_EDGE('',*,*,#8700,.F.);
#13849=ORIENTED_EDGE('',*,*,#9623,.F.);
#13850=ORIENTED_EDGE('',*,*,#8715,.T.);
#13851=ORIENTED_EDGE('',*,*,#8732,.F.);
#13852=ORIENTED_EDGE('',*,*,#8726,.F.);
#13853=ORIENTED_EDGE('',*,*,#9622,.F.);
#13854=ORIENTED_EDGE('',*,*,#8595,.T.);
#13855=ORIENTED_EDGE('',*,*,#8593,.F.);
#13856=ORIENTED_EDGE('',*,*,#8586,.F.);
#13857=ORIENTED_EDGE('',*,*,#9621,.F.);
#13858=ORIENTED_EDGE('',*,*,#8610,.T.);
#13859=ORIENTED_EDGE('',*,*,#8608,.F.);
#13860=ORIENTED_EDGE('',*,*,#8602,.F.);
#13861=ORIENTED_EDGE('',*,*,#9620,.F.);
#13862=ORIENTED_EDGE('',*,*,#8624,.T.);
#13863=ORIENTED_EDGE('',*,*,#8622,.F.);
#13864=ORIENTED_EDGE('',*,*,#8615,.F.);
#13865=ORIENTED_EDGE('',*,*,#9619,.F.);
#13866=ORIENTED_EDGE('',*,*,#8647,.T.);
#13867=ORIENTED_EDGE('',*,*,#8636,.F.);
#13868=ORIENTED_EDGE('',*,*,#8629,.F.);
#13869=ORIENTED_EDGE('',*,*,#8483,.F.);
#13870=ORIENTED_EDGE('',*,*,#8487,.T.);
#13871=ORIENTED_EDGE('',*,*,#8406,.F.);
#13872=ORIENTED_EDGE('',*,*,#8645,.T.);
#13873=ORIENTED_EDGE('',*,*,#8641,.F.);
#13874=ORIENTED_EDGE('',*,*,#9726,.T.);
#13875=ORIENTED_EDGE('',*,*,#9618,.F.);
#13876=ORIENTED_EDGE('',*,*,#8480,.T.);
#13877=ORIENTED_EDGE('',*,*,#9726,.F.);
#13878=ORIENTED_EDGE('',*,*,#8640,.F.);
#13879=ORIENTED_EDGE('',*,*,#9617,.F.);
#13880=ORIENTED_EDGE('',*,*,#8493,.T.);
#13881=ORIENTED_EDGE('',*,*,#8583,.F.);
#13882=ORIENTED_EDGE('',*,*,#8490,.F.);
#13883=ORIENTED_EDGE('',*,*,#9616,.F.);
#13884=ORIENTED_EDGE('',*,*,#8507,.T.);
#13885=ORIENTED_EDGE('',*,*,#8582,.F.);
#13886=ORIENTED_EDGE('',*,*,#8504,.F.);
#13887=ORIENTED_EDGE('',*,*,#9615,.F.);
#13888=ORIENTED_EDGE('',*,*,#8521,.T.);
#13889=ORIENTED_EDGE('',*,*,#8581,.F.);
#13890=ORIENTED_EDGE('',*,*,#8518,.F.);
#13891=ORIENTED_EDGE('',*,*,#9614,.F.);
#13892=ORIENTED_EDGE('',*,*,#8535,.T.);
#13893=ORIENTED_EDGE('',*,*,#8580,.F.);
#13894=ORIENTED_EDGE('',*,*,#8532,.F.);
#13895=ORIENTED_EDGE('',*,*,#9613,.F.);
#13896=ORIENTED_EDGE('',*,*,#8549,.T.);
#13897=ORIENTED_EDGE('',*,*,#8579,.F.);
#13898=ORIENTED_EDGE('',*,*,#8546,.F.);
#13899=ORIENTED_EDGE('',*,*,#9612,.F.);
#13900=ORIENTED_EDGE('',*,*,#8561,.T.);
#13901=ORIENTED_EDGE('',*,*,#8578,.F.);
#13902=ORIENTED_EDGE('',*,*,#8571,.F.);
#13903=ORIENTED_EDGE('',*,*,#9611,.F.);
#13904=ORIENTED_EDGE('',*,*,#8444,.T.);
#13905=ORIENTED_EDGE('',*,*,#8442,.F.);
#13906=ORIENTED_EDGE('',*,*,#8435,.F.);
#13907=ORIENTED_EDGE('',*,*,#9610,.F.);
#13908=ORIENTED_EDGE('',*,*,#8458,.T.);
#13909=ORIENTED_EDGE('',*,*,#8456,.F.);
#13910=ORIENTED_EDGE('',*,*,#8449,.F.);
#13911=ORIENTED_EDGE('',*,*,#9609,.F.);
#13912=ORIENTED_EDGE('',*,*,#8479,.T.);
#13913=ORIENTED_EDGE('',*,*,#8470,.F.);
#13914=ORIENTED_EDGE('',*,*,#8463,.F.);
#13915=ORIENTED_EDGE('',*,*,#9608,.F.);
#13916=ORIENTED_EDGE('',*,*,#8065,.T.);
#13917=ORIENTED_EDGE('',*,*,#8070,.F.);
#13918=ORIENTED_EDGE('',*,*,#8474,.F.);
#13919=ORIENTED_EDGE('',*,*,#9607,.F.);
#13920=ORIENTED_EDGE('',*,*,#8083,.T.);
#13921=ORIENTED_EDGE('',*,*,#8088,.F.);
#13922=ORIENTED_EDGE('',*,*,#8055,.F.);
#13923=ORIENTED_EDGE('',*,*,#9605,.F.);
#13924=ORIENTED_EDGE('',*,*,#8104,.T.);
#13925=ORIENTED_EDGE('',*,*,#8081,.F.);
#13926=ORIENTED_EDGE('',*,*,#8073,.F.);
#13927=ORIENTED_EDGE('',*,*,#9603,.F.);
#13928=ORIENTED_EDGE('',*,*,#8107,.T.);
#13929=ORIENTED_EDGE('',*,*,#8102,.F.);
#13930=ORIENTED_EDGE('',*,*,#8094,.F.);
#13931=ORIENTED_EDGE('',*,*,#9601,.F.);
#13932=ORIENTED_EDGE('',*,*,#9521,.T.);
#13933=ORIENTED_EDGE('',*,*,#8428,.F.);
#13934=ORIENTED_EDGE('',*,*,#8432,.F.);
#13935=ORIENTED_EDGE('',*,*,#9599,.F.);
#13936=ORIENTED_EDGE('',*,*,#9545,.T.);
#13937=ORIENTED_EDGE('',*,*,#9530,.F.);
#13938=ORIENTED_EDGE('',*,*,#9528,.F.);
#13939=ORIENTED_EDGE('',*,*,#9597,.F.);
#13940=ORIENTED_EDGE('',*,*,#9569,.T.);
#13941=ORIENTED_EDGE('',*,*,#9554,.F.);
#13942=ORIENTED_EDGE('',*,*,#9552,.F.);
#13943=ORIENTED_EDGE('',*,*,#9595,.F.);
#13944=ORIENTED_EDGE('',*,*,#9581,.T.);
#13945=ORIENTED_EDGE('',*,*,#9578,.F.);
#13946=ORIENTED_EDGE('',*,*,#9576,.F.);
#13947=ORIENTED_EDGE('',*,*,#9693,.F.);
#13948=ORIENTED_EDGE('',*,*,#9558,.T.);
#13949=ORIENTED_EDGE('',*,*,#9568,.F.);
#13950=ORIENTED_EDGE('',*,*,#9587,.F.);
#13951=ORIENTED_EDGE('',*,*,#9593,.F.);
#13952=ORIENTED_EDGE('',*,*,#9691,.F.);
#13953=ORIENTED_EDGE('',*,*,#9534,.T.);
#13954=ORIENTED_EDGE('',*,*,#9544,.F.);
#13955=ORIENTED_EDGE('',*,*,#9565,.F.);
#13956=ORIENTED_EDGE('',*,*,#9689,.F.);
#13957=ORIENTED_EDGE('',*,*,#8110,.T.);
#13958=ORIENTED_EDGE('',*,*,#8118,.F.);
#13959=ORIENTED_EDGE('',*,*,#9541,.F.);
#13960=ORIENTED_EDGE('',*,*,#9687,.F.);
#13961=ORIENTED_EDGE('',*,*,#9499,.T.);
#13962=ORIENTED_EDGE('',*,*,#9520,.F.);
#13963=ORIENTED_EDGE('',*,*,#9518,.F.);
#13964=ORIENTED_EDGE('',*,*,#9686,.F.);
#13965=ORIENTED_EDGE('',*,*,#8135,.T.);
#13966=ORIENTED_EDGE('',*,*,#9516,.F.);
#13967=ORIENTED_EDGE('',*,*,#8125,.F.);
#13968=ORIENTED_EDGE('',*,*,#9685,.F.);
#13969=ORIENTED_EDGE('',*,*,#8150,.T.);
#13970=ORIENTED_EDGE('',*,*,#9515,.F.);
#13971=ORIENTED_EDGE('',*,*,#8147,.F.);
#13972=ORIENTED_EDGE('',*,*,#9684,.F.);
#13973=ORIENTED_EDGE('',*,*,#8165,.T.);
#13974=ORIENTED_EDGE('',*,*,#9514,.F.);
#13975=ORIENTED_EDGE('',*,*,#8162,.F.);
#13976=ORIENTED_EDGE('',*,*,#9683,.F.);
#13977=ORIENTED_EDGE('',*,*,#8180,.T.);
#13978=ORIENTED_EDGE('',*,*,#9513,.F.);
#13979=ORIENTED_EDGE('',*,*,#8177,.F.);
#13980=ORIENTED_EDGE('',*,*,#9682,.F.);
#13981=ORIENTED_EDGE('',*,*,#8195,.T.);
#13982=ORIENTED_EDGE('',*,*,#9512,.F.);
#13983=ORIENTED_EDGE('',*,*,#8192,.F.);
#13984=ORIENTED_EDGE('',*,*,#9681,.F.);
#13985=ORIENTED_EDGE('',*,*,#8210,.T.);
#13986=ORIENTED_EDGE('',*,*,#9511,.F.);
#13987=ORIENTED_EDGE('',*,*,#8207,.F.);
#13988=ORIENTED_EDGE('',*,*,#9680,.F.);
#13989=ORIENTED_EDGE('',*,*,#8225,.T.);
#13990=ORIENTED_EDGE('',*,*,#9510,.F.);
#13991=ORIENTED_EDGE('',*,*,#8222,.F.);
#13992=ORIENTED_EDGE('',*,*,#9679,.F.);
#13993=ORIENTED_EDGE('',*,*,#8240,.T.);
#13994=ORIENTED_EDGE('',*,*,#9509,.F.);
#13995=ORIENTED_EDGE('',*,*,#8237,.F.);
#13996=ORIENTED_EDGE('',*,*,#9678,.F.);
#13997=ORIENTED_EDGE('',*,*,#9349,.T.);
#13998=ORIENTED_EDGE('',*,*,#9508,.F.);
#13999=ORIENTED_EDGE('',*,*,#8252,.F.);
#14000=ORIENTED_EDGE('',*,*,#9677,.F.);
#14001=ORIENTED_EDGE('',*,*,#9361,.T.);
#14002=ORIENTED_EDGE('',*,*,#9493,.F.);
#14003=ORIENTED_EDGE('',*,*,#9358,.F.);
#14004=ORIENTED_EDGE('',*,*,#9676,.F.);
#14005=ORIENTED_EDGE('',*,*,#9375,.T.);
#14006=ORIENTED_EDGE('',*,*,#9492,.F.);
#14007=ORIENTED_EDGE('',*,*,#9372,.F.);
#14008=ORIENTED_EDGE('',*,*,#9675,.F.);
#14009=ORIENTED_EDGE('',*,*,#9389,.T.);
#14010=ORIENTED_EDGE('',*,*,#9491,.F.);
#14011=ORIENTED_EDGE('',*,*,#9386,.F.);
#14012=ORIENTED_EDGE('',*,*,#9674,.F.);
#14013=ORIENTED_EDGE('',*,*,#9403,.T.);
#14014=ORIENTED_EDGE('',*,*,#9490,.F.);
#14015=ORIENTED_EDGE('',*,*,#9400,.F.);
#14016=ORIENTED_EDGE('',*,*,#9673,.F.);
#14017=ORIENTED_EDGE('',*,*,#9417,.T.);
#14018=ORIENTED_EDGE('',*,*,#9489,.F.);
#14019=ORIENTED_EDGE('',*,*,#9414,.F.);
#14020=ORIENTED_EDGE('',*,*,#9672,.F.);
#14021=ORIENTED_EDGE('',*,*,#9431,.T.);
#14022=ORIENTED_EDGE('',*,*,#9488,.F.);
#14023=ORIENTED_EDGE('',*,*,#9428,.F.);
#14024=ORIENTED_EDGE('',*,*,#9671,.F.);
#14025=ORIENTED_EDGE('',*,*,#9445,.T.);
#14026=ORIENTED_EDGE('',*,*,#9487,.F.);
#14027=ORIENTED_EDGE('',*,*,#9442,.F.);
#14028=ORIENTED_EDGE('',*,*,#9670,.F.);
#14029=ORIENTED_EDGE('',*,*,#9459,.T.);
#14030=ORIENTED_EDGE('',*,*,#9486,.F.);
#14031=ORIENTED_EDGE('',*,*,#9456,.F.);
#14032=ORIENTED_EDGE('',*,*,#9669,.F.);
#14033=ORIENTED_EDGE('',*,*,#9470,.T.);
#14034=ORIENTED_EDGE('',*,*,#9475,.F.);
#14035=ORIENTED_EDGE('',*,*,#9477,.F.);
#14036=ORIENTED_EDGE('',*,*,#9668,.F.);
#14037=ORIENTED_EDGE('',*,*,#9315,.T.);
#14038=ORIENTED_EDGE('',*,*,#9727,.F.);
#14039=ORIENTED_EDGE('',*,*,#8044,.F.);
#14040=ORIENTED_EDGE('',*,*,#8045,.F.);
#14041=ORIENTED_EDGE('',*,*,#9727,.T.);
#14042=ORIENTED_EDGE('',*,*,#9318,.F.);
#14043=ORIENTED_EDGE('',*,*,#9322,.T.);
#14044=ORIENTED_EDGE('',*,*,#8306,.F.);
#14045=ORIENTED_EDGE('',*,*,#8049,.T.);
#14046=ORIENTED_EDGE('',*,*,#9667,.F.);
#14047=ORIENTED_EDGE('',*,*,#9326,.T.);
#14048=ORIENTED_EDGE('',*,*,#9348,.F.);
#14049=ORIENTED_EDGE('',*,*,#9346,.F.);
#14050=ORIENTED_EDGE('',*,*,#9666,.F.);
#14051=ORIENTED_EDGE('',*,*,#9207,.T.);
#14052=ORIENTED_EDGE('',*,*,#9205,.F.);
#14053=ORIENTED_EDGE('',*,*,#9198,.F.);
#14054=ORIENTED_EDGE('',*,*,#9665,.F.);
#14055=ORIENTED_EDGE('',*,*,#9221,.T.);
#14056=ORIENTED_EDGE('',*,*,#9219,.F.);
#14057=ORIENTED_EDGE('',*,*,#9212,.F.);
#14058=ORIENTED_EDGE('',*,*,#9664,.F.);
#14059=ORIENTED_EDGE('',*,*,#9235,.T.);
#14060=ORIENTED_EDGE('',*,*,#9233,.F.);
#14061=ORIENTED_EDGE('',*,*,#9226,.F.);
#14062=ORIENTED_EDGE('',*,*,#9663,.F.);
#14063=ORIENTED_EDGE('',*,*,#9249,.T.);
#14064=ORIENTED_EDGE('',*,*,#9247,.F.);
#14065=ORIENTED_EDGE('',*,*,#9240,.F.);
#14066=ORIENTED_EDGE('',*,*,#9662,.F.);
#14067=ORIENTED_EDGE('',*,*,#9263,.T.);
#14068=ORIENTED_EDGE('',*,*,#9261,.F.);
#14069=ORIENTED_EDGE('',*,*,#9254,.F.);
#14070=ORIENTED_EDGE('',*,*,#9661,.F.);
#14071=ORIENTED_EDGE('',*,*,#9277,.T.);
#14072=ORIENTED_EDGE('',*,*,#9275,.F.);
#14073=ORIENTED_EDGE('',*,*,#9268,.F.);
#14074=ORIENTED_EDGE('',*,*,#9660,.F.);
#14075=ORIENTED_EDGE('',*,*,#9291,.T.);
#14076=ORIENTED_EDGE('',*,*,#9289,.F.);
#14077=ORIENTED_EDGE('',*,*,#9282,.F.);
#14078=ORIENTED_EDGE('',*,*,#9659,.F.);
#14079=ORIENTED_EDGE('',*,*,#9314,.T.);
#14080=ORIENTED_EDGE('',*,*,#9303,.F.);
#14081=ORIENTED_EDGE('',*,*,#9296,.F.);
#14082=ORIENTED_EDGE('',*,*,#9151,.F.);
#14083=ORIENTED_EDGE('',*,*,#9155,.T.);
#14084=ORIENTED_EDGE('',*,*,#8326,.F.);
#14085=ORIENTED_EDGE('',*,*,#9312,.T.);
#14086=ORIENTED_EDGE('',*,*,#9308,.F.);
#14087=ORIENTED_EDGE('',*,*,#9728,.T.);
#14088=ORIENTED_EDGE('',*,*,#9658,.F.);
#14089=ORIENTED_EDGE('',*,*,#9148,.T.);
#14090=ORIENTED_EDGE('',*,*,#9728,.F.);
#14091=ORIENTED_EDGE('',*,*,#9307,.F.);
#14092=ORIENTED_EDGE('',*,*,#9657,.F.);
#14093=ORIENTED_EDGE('',*,*,#9161,.T.);
#14094=ORIENTED_EDGE('',*,*,#9195,.F.);
#14095=ORIENTED_EDGE('',*,*,#9158,.F.);
#14096=ORIENTED_EDGE('',*,*,#9656,.F.);
#14097=ORIENTED_EDGE('',*,*,#9173,.T.);
#14098=ORIENTED_EDGE('',*,*,#9194,.F.);
#14099=ORIENTED_EDGE('',*,*,#9191,.F.);
#14100=ORIENTED_EDGE('',*,*,#9655,.F.);
#14101=ORIENTED_EDGE('',*,*,#9054,.T.);
#14102=ORIENTED_EDGE('',*,*,#9052,.F.);
#14103=ORIENTED_EDGE('',*,*,#9045,.F.);
#14104=ORIENTED_EDGE('',*,*,#9654,.F.);
#14105=ORIENTED_EDGE('',*,*,#9068,.T.);
#14106=ORIENTED_EDGE('',*,*,#9066,.F.);
#14107=ORIENTED_EDGE('',*,*,#9059,.F.);
#14108=ORIENTED_EDGE('',*,*,#9653,.F.);
#14109=ORIENTED_EDGE('',*,*,#9082,.T.);
#14110=ORIENTED_EDGE('',*,*,#9080,.F.);
#14111=ORIENTED_EDGE('',*,*,#9073,.F.);
#14112=ORIENTED_EDGE('',*,*,#9652,.F.);
#14113=ORIENTED_EDGE('',*,*,#9096,.T.);
#14114=ORIENTED_EDGE('',*,*,#9094,.F.);
#14115=ORIENTED_EDGE('',*,*,#9087,.F.);
#14116=ORIENTED_EDGE('',*,*,#9651,.F.);
#14117=ORIENTED_EDGE('',*,*,#9110,.T.);
#14118=ORIENTED_EDGE('',*,*,#9108,.F.);
#14119=ORIENTED_EDGE('',*,*,#9101,.F.);
#14120=ORIENTED_EDGE('',*,*,#9650,.F.);
#14121=ORIENTED_EDGE('',*,*,#9124,.T.);
#14122=ORIENTED_EDGE('',*,*,#9122,.F.);
#14123=ORIENTED_EDGE('',*,*,#9115,.F.);
#14124=ORIENTED_EDGE('',*,*,#9649,.F.);
#14125=ORIENTED_EDGE('',*,*,#9147,.T.);
#14126=ORIENTED_EDGE('',*,*,#9136,.F.);
#14127=ORIENTED_EDGE('',*,*,#9129,.F.);
#14128=ORIENTED_EDGE('',*,*,#8985,.F.);
#14129=ORIENTED_EDGE('',*,*,#8989,.T.);
#14130=ORIENTED_EDGE('',*,*,#8346,.F.);
#14131=ORIENTED_EDGE('',*,*,#9145,.T.);
#14132=ORIENTED_EDGE('',*,*,#9141,.F.);
#14133=ORIENTED_EDGE('',*,*,#9729,.T.);
#14134=ORIENTED_EDGE('',*,*,#9648,.F.);
#14135=ORIENTED_EDGE('',*,*,#8982,.T.);
#14136=ORIENTED_EDGE('',*,*,#9729,.F.);
#14137=ORIENTED_EDGE('',*,*,#9140,.F.);
#14138=ORIENTED_EDGE('',*,*,#9647,.F.);
#14139=ORIENTED_EDGE('',*,*,#8995,.T.);
#14140=ORIENTED_EDGE('',*,*,#9042,.F.);
#14141=ORIENTED_EDGE('',*,*,#8992,.F.);
#14142=ORIENTED_EDGE('',*,*,#9646,.F.);
#14143=ORIENTED_EDGE('',*,*,#9009,.T.);
#14144=ORIENTED_EDGE('',*,*,#9041,.F.);
#14145=ORIENTED_EDGE('',*,*,#9006,.F.);
#14146=ORIENTED_EDGE('',*,*,#9645,.F.);
#14147=ORIENTED_EDGE('',*,*,#9021,.T.);
#14148=ORIENTED_EDGE('',*,*,#9040,.F.);
#14149=ORIENTED_EDGE('',*,*,#9036,.F.);
#14150=ORIENTED_EDGE('',*,*,#9730,.F.);
#14151=ORIENTED_EDGE('',*,*,#9731,.T.);
#14152=ORIENTED_EDGE('',*,*,#9731,.F.);
#14153=ORIENTED_EDGE('',*,*,#9732,.F.);
#14154=ORIENTED_EDGE('',*,*,#9733,.T.);
#14155=ORIENTED_EDGE('',*,*,#9733,.F.);
#14156=ORIENTED_EDGE('',*,*,#9734,.F.);
#14157=ORIENTED_EDGE('',*,*,#9735,.T.);
#14158=ORIENTED_EDGE('',*,*,#9735,.F.);
#14159=ORIENTED_EDGE('',*,*,#9736,.F.);
#14160=ORIENTED_EDGE('',*,*,#9737,.T.);
#14161=ORIENTED_EDGE('',*,*,#9737,.F.);
#14162=ORIENTED_EDGE('',*,*,#9738,.F.);
#14163=ORIENTED_EDGE('',*,*,#9739,.T.);
#14164=ORIENTED_EDGE('',*,*,#9739,.F.);
#14165=ORIENTED_EDGE('',*,*,#9700,.F.);
#14166=ORIENTED_EDGE('',*,*,#9740,.T.);
#14167=ORIENTED_EDGE('',*,*,#9741,.F.);
#14168=ORIENTED_EDGE('',*,*,#9740,.F.);
#14169=ORIENTED_EDGE('',*,*,#9496,.T.);
#14170=ORIENTED_EDGE('',*,*,#9720,.T.);
#14171=ORIENTED_EDGE('',*,*,#9716,.T.);
#14172=ORIENTED_EDGE('',*,*,#9712,.T.);
#14173=ORIENTED_EDGE('',*,*,#9708,.T.);
#14174=ORIENTED_EDGE('',*,*,#9704,.T.);
#14175=ORIENTED_EDGE('',*,*,#9741,.T.);
#14176=ORIENTED_EDGE('',*,*,#9738,.T.);
#14177=ORIENTED_EDGE('',*,*,#9736,.T.);
#14178=ORIENTED_EDGE('',*,*,#9734,.T.);
#14179=ORIENTED_EDGE('',*,*,#9732,.T.);
#14180=ORIENTED_EDGE('',*,*,#9730,.T.);
#14181=ORIENTED_EDGE('',*,*,#9742,.T.);
#14182=ORIENTED_EDGE('',*,*,#9743,.T.);
#14183=ORIENTED_EDGE('',*,*,#9744,.F.);
#14184=ORIENTED_EDGE('',*,*,#9745,.T.);
#14185=ORIENTED_EDGE('',*,*,#9746,.T.);
#14186=ORIENTED_EDGE('',*,*,#9747,.T.);
#14187=ORIENTED_EDGE('',*,*,#9742,.F.);
#14188=ORIENTED_EDGE('',*,*,#9748,.T.);
#14189=ORIENTED_EDGE('',*,*,#9749,.T.);
#14190=ORIENTED_EDGE('',*,*,#9750,.T.);
#14191=ORIENTED_EDGE('',*,*,#9746,.F.);
#14192=ORIENTED_EDGE('',*,*,#9751,.T.);
#14193=ORIENTED_EDGE('',*,*,#9752,.T.);
#14194=ORIENTED_EDGE('',*,*,#9753,.T.);
#14195=ORIENTED_EDGE('',*,*,#9749,.F.);
#14196=ORIENTED_EDGE('',*,*,#9754,.T.);
#14197=ORIENTED_EDGE('',*,*,#9755,.T.);
#14198=ORIENTED_EDGE('',*,*,#9756,.T.);
#14199=ORIENTED_EDGE('',*,*,#9752,.F.);
#14200=ORIENTED_EDGE('',*,*,#9757,.T.);
#14201=ORIENTED_EDGE('',*,*,#9758,.T.);
#14202=ORIENTED_EDGE('',*,*,#9759,.T.);
#14203=ORIENTED_EDGE('',*,*,#9755,.F.);
#14204=ORIENTED_EDGE('',*,*,#9760,.T.);
#14205=ORIENTED_EDGE('',*,*,#9761,.T.);
#14206=ORIENTED_EDGE('',*,*,#9762,.T.);
#14207=ORIENTED_EDGE('',*,*,#9758,.F.);
#14208=ORIENTED_EDGE('',*,*,#9763,.T.);
#14209=ORIENTED_EDGE('',*,*,#9764,.T.);
#14210=ORIENTED_EDGE('',*,*,#9765,.T.);
#14211=ORIENTED_EDGE('',*,*,#9761,.F.);
#14212=ORIENTED_EDGE('',*,*,#9766,.T.);
#14213=ORIENTED_EDGE('',*,*,#9767,.T.);
#14214=ORIENTED_EDGE('',*,*,#9768,.T.);
#14215=ORIENTED_EDGE('',*,*,#9764,.F.);
#14216=ORIENTED_EDGE('',*,*,#9769,.T.);
#14217=ORIENTED_EDGE('',*,*,#9770,.T.);
#14218=ORIENTED_EDGE('',*,*,#9771,.T.);
#14219=ORIENTED_EDGE('',*,*,#9767,.F.);
#14220=ORIENTED_EDGE('',*,*,#9772,.T.);
#14221=ORIENTED_EDGE('',*,*,#9773,.T.);
#14222=ORIENTED_EDGE('',*,*,#9774,.T.);
#14223=ORIENTED_EDGE('',*,*,#9770,.F.);
#14224=ORIENTED_EDGE('',*,*,#9775,.T.);
#14225=ORIENTED_EDGE('',*,*,#9776,.F.);
#14226=ORIENTED_EDGE('',*,*,#9777,.T.);
#14227=ORIENTED_EDGE('',*,*,#9778,.T.);
#14228=ORIENTED_EDGE('',*,*,#9779,.T.);
#14229=ORIENTED_EDGE('',*,*,#9780,.T.);
#14230=ORIENTED_EDGE('',*,*,#9781,.T.);
#14231=ORIENTED_EDGE('',*,*,#9782,.F.);
#14232=ORIENTED_EDGE('',*,*,#9783,.F.);
#14233=ORIENTED_EDGE('',*,*,#9784,.T.);
#14234=ORIENTED_EDGE('',*,*,#9785,.T.);
#14235=ORIENTED_EDGE('',*,*,#9780,.F.);
#14236=ORIENTED_EDGE('',*,*,#9786,.F.);
#14237=ORIENTED_EDGE('',*,*,#9787,.T.);
#14238=ORIENTED_EDGE('',*,*,#9788,.T.);
#14239=ORIENTED_EDGE('',*,*,#9784,.F.);
#14240=ORIENTED_EDGE('',*,*,#9789,.F.);
#14241=ORIENTED_EDGE('',*,*,#9790,.T.);
#14242=ORIENTED_EDGE('',*,*,#9791,.T.);
#14243=ORIENTED_EDGE('',*,*,#9787,.F.);
#14244=ORIENTED_EDGE('',*,*,#9792,.F.);
#14245=ORIENTED_EDGE('',*,*,#9793,.T.);
#14246=ORIENTED_EDGE('',*,*,#9794,.T.);
#14247=ORIENTED_EDGE('',*,*,#9790,.F.);
#14248=ORIENTED_EDGE('',*,*,#9795,.F.);
#14249=ORIENTED_EDGE('',*,*,#9796,.T.);
#14250=ORIENTED_EDGE('',*,*,#9797,.T.);
#14251=ORIENTED_EDGE('',*,*,#9793,.F.);
#14252=ORIENTED_EDGE('',*,*,#9798,.F.);
#14253=ORIENTED_EDGE('',*,*,#9799,.T.);
#14254=ORIENTED_EDGE('',*,*,#9800,.T.);
#14255=ORIENTED_EDGE('',*,*,#9796,.F.);
#14256=ORIENTED_EDGE('',*,*,#9801,.F.);
#14257=ORIENTED_EDGE('',*,*,#9802,.T.);
#14258=ORIENTED_EDGE('',*,*,#9803,.T.);
#14259=ORIENTED_EDGE('',*,*,#9799,.F.);
#14260=ORIENTED_EDGE('',*,*,#9804,.F.);
#14261=ORIENTED_EDGE('',*,*,#9805,.T.);
#14262=ORIENTED_EDGE('',*,*,#9806,.T.);
#14263=ORIENTED_EDGE('',*,*,#9802,.F.);
#14264=ORIENTED_EDGE('',*,*,#9807,.F.);
#14265=ORIENTED_EDGE('',*,*,#9808,.T.);
#14266=ORIENTED_EDGE('',*,*,#9809,.T.);
#14267=ORIENTED_EDGE('',*,*,#9805,.F.);
#14268=ORIENTED_EDGE('',*,*,#9810,.F.);
#14269=ORIENTED_EDGE('',*,*,#9811,.T.);
#14270=ORIENTED_EDGE('',*,*,#9812,.T.);
#14271=ORIENTED_EDGE('',*,*,#9808,.F.);
#14272=ORIENTED_EDGE('',*,*,#9813,.F.);
#14273=ORIENTED_EDGE('',*,*,#9814,.F.);
#14274=ORIENTED_EDGE('',*,*,#9815,.F.);
#14275=ORIENTED_EDGE('',*,*,#9816,.F.);
#14276=ORIENTED_EDGE('',*,*,#9817,.T.);
#14277=ORIENTED_EDGE('',*,*,#9814,.T.);
#14278=ORIENTED_EDGE('',*,*,#9818,.T.);
#14279=ORIENTED_EDGE('',*,*,#9811,.F.);
#14280=ORIENTED_EDGE('',*,*,#9819,.F.);
#14281=ORIENTED_EDGE('',*,*,#9820,.F.);
#14282=ORIENTED_EDGE('',*,*,#9781,.F.);
#14283=ORIENTED_EDGE('',*,*,#9785,.F.);
#14284=ORIENTED_EDGE('',*,*,#9788,.F.);
#14285=ORIENTED_EDGE('',*,*,#9791,.F.);
#14286=ORIENTED_EDGE('',*,*,#9794,.F.);
#14287=ORIENTED_EDGE('',*,*,#9797,.F.);
#14288=ORIENTED_EDGE('',*,*,#9800,.F.);
#14289=ORIENTED_EDGE('',*,*,#9803,.F.);
#14290=ORIENTED_EDGE('',*,*,#9806,.F.);
#14291=ORIENTED_EDGE('',*,*,#9809,.F.);
#14292=ORIENTED_EDGE('',*,*,#9812,.F.);
#14293=ORIENTED_EDGE('',*,*,#9818,.F.);
#14294=ORIENTED_EDGE('',*,*,#9817,.F.);
#14295=ORIENTED_EDGE('',*,*,#9821,.F.);
#14296=ORIENTED_EDGE('',*,*,#9743,.F.);
#14297=ORIENTED_EDGE('',*,*,#9747,.F.);
#14298=ORIENTED_EDGE('',*,*,#9750,.F.);
#14299=ORIENTED_EDGE('',*,*,#9753,.F.);
#14300=ORIENTED_EDGE('',*,*,#9756,.F.);
#14301=ORIENTED_EDGE('',*,*,#9759,.F.);
#14302=ORIENTED_EDGE('',*,*,#9762,.F.);
#14303=ORIENTED_EDGE('',*,*,#9765,.F.);
#14304=ORIENTED_EDGE('',*,*,#9768,.F.);
#14305=ORIENTED_EDGE('',*,*,#9771,.F.);
#14306=ORIENTED_EDGE('',*,*,#9774,.F.);
#14307=ORIENTED_EDGE('',*,*,#9822,.F.);
#14308=ORIENTED_EDGE('',*,*,#9779,.F.);
#14309=ORIENTED_EDGE('',*,*,#9823,.F.);
#14310=ORIENTED_EDGE('',*,*,#9777,.F.);
#14311=ORIENTED_EDGE('',*,*,#9824,.F.);
#14312=ORIENTED_EDGE('',*,*,#9775,.F.);
#14313=ORIENTED_EDGE('',*,*,#9772,.F.);
#14314=ORIENTED_EDGE('',*,*,#9769,.F.);
#14315=ORIENTED_EDGE('',*,*,#9766,.F.);
#14316=ORIENTED_EDGE('',*,*,#9763,.F.);
#14317=ORIENTED_EDGE('',*,*,#9760,.F.);
#14318=ORIENTED_EDGE('',*,*,#9757,.F.);
#14319=ORIENTED_EDGE('',*,*,#9754,.F.);
#14320=ORIENTED_EDGE('',*,*,#9751,.F.);
#14321=ORIENTED_EDGE('',*,*,#9748,.F.);
#14322=ORIENTED_EDGE('',*,*,#9745,.F.);
#14323=ORIENTED_EDGE('',*,*,#9825,.F.);
#14324=ORIENTED_EDGE('',*,*,#9815,.T.);
#14325=ORIENTED_EDGE('',*,*,#9819,.T.);
#14326=ORIENTED_EDGE('',*,*,#9813,.T.);
#14327=ORIENTED_EDGE('',*,*,#9810,.T.);
#14328=ORIENTED_EDGE('',*,*,#9807,.T.);
#14329=ORIENTED_EDGE('',*,*,#9804,.T.);
#14330=ORIENTED_EDGE('',*,*,#9801,.T.);
#14331=ORIENTED_EDGE('',*,*,#9798,.T.);
#14332=ORIENTED_EDGE('',*,*,#9795,.T.);
#14333=ORIENTED_EDGE('',*,*,#9792,.T.);
#14334=ORIENTED_EDGE('',*,*,#9789,.T.);
#14335=ORIENTED_EDGE('',*,*,#9786,.T.);
#14336=ORIENTED_EDGE('',*,*,#9783,.T.);
#14337=ORIENTED_EDGE('',*,*,#9826,.F.);
#14338=ORIENTED_EDGE('',*,*,#9821,.T.);
#14339=ORIENTED_EDGE('',*,*,#9816,.T.);
#14340=ORIENTED_EDGE('',*,*,#9825,.T.);
#14341=ORIENTED_EDGE('',*,*,#9744,.T.);
#14342=ORIENTED_EDGE('',*,*,#9776,.T.);
#14343=ORIENTED_EDGE('',*,*,#9822,.T.);
#14344=ORIENTED_EDGE('',*,*,#9773,.F.);
#14345=ORIENTED_EDGE('',*,*,#9824,.T.);
#14346=ORIENTED_EDGE('',*,*,#9827,.F.);
#14347=ORIENTED_EDGE('',*,*,#9828,.T.);
#14348=ORIENTED_EDGE('',*,*,#9826,.T.);
#14349=ORIENTED_EDGE('',*,*,#9828,.F.);
#14350=ORIENTED_EDGE('',*,*,#9829,.F.);
#14351=ORIENTED_EDGE('',*,*,#9827,.T.);
#14352=ORIENTED_EDGE('',*,*,#9830,.F.);
#14353=ORIENTED_EDGE('',*,*,#9831,.T.);
#14354=ORIENTED_EDGE('',*,*,#9829,.T.);
#14355=ORIENTED_EDGE('',*,*,#9831,.F.);
#14356=ORIENTED_EDGE('',*,*,#9832,.F.);
#14357=ORIENTED_EDGE('',*,*,#9833,.T.);
#14358=ORIENTED_EDGE('',*,*,#9830,.T.);
#14359=ORIENTED_EDGE('',*,*,#9833,.F.);
#14360=ORIENTED_EDGE('',*,*,#9832,.T.);
#14361=ORIENTED_EDGE('',*,*,#9820,.T.);
#14362=ORIENTED_EDGE('',*,*,#9778,.F.);
#14363=ORIENTED_EDGE('',*,*,#9823,.T.);
#14364=ORIENTED_EDGE('',*,*,#9782,.T.);
#14365=ORIENTED_EDGE('',*,*,#9834,.F.);
#14366=ORIENTED_EDGE('',*,*,#9835,.T.);
#14367=ORIENTED_EDGE('',*,*,#9836,.T.);
#14368=ORIENTED_EDGE('',*,*,#9837,.T.);
#14369=ORIENTED_EDGE('',*,*,#9838,.F.);
#14370=ORIENTED_EDGE('',*,*,#9839,.T.);
#14371=ORIENTED_EDGE('',*,*,#9834,.T.);
#14372=ORIENTED_EDGE('',*,*,#9840,.T.);
#14373=ORIENTED_EDGE('',*,*,#9841,.F.);
#14374=ORIENTED_EDGE('',*,*,#9842,.T.);
#14375=ORIENTED_EDGE('',*,*,#9838,.T.);
#14376=ORIENTED_EDGE('',*,*,#9843,.T.);
#14377=ORIENTED_EDGE('',*,*,#9844,.F.);
#14378=ORIENTED_EDGE('',*,*,#9845,.T.);
#14379=ORIENTED_EDGE('',*,*,#9841,.T.);
#14380=ORIENTED_EDGE('',*,*,#9846,.T.);
#14381=ORIENTED_EDGE('',*,*,#9847,.F.);
#14382=ORIENTED_EDGE('',*,*,#9848,.T.);
#14383=ORIENTED_EDGE('',*,*,#9844,.T.);
#14384=ORIENTED_EDGE('',*,*,#9849,.T.);
#14385=ORIENTED_EDGE('',*,*,#9850,.F.);
#14386=ORIENTED_EDGE('',*,*,#9851,.T.);
#14387=ORIENTED_EDGE('',*,*,#9847,.T.);
#14388=ORIENTED_EDGE('',*,*,#9852,.T.);
#14389=ORIENTED_EDGE('',*,*,#9853,.F.);
#14390=ORIENTED_EDGE('',*,*,#9854,.T.);
#14391=ORIENTED_EDGE('',*,*,#9855,.F.);
#14392=ORIENTED_EDGE('',*,*,#9856,.F.);
#14393=ORIENTED_EDGE('',*,*,#9857,.F.);
#14394=ORIENTED_EDGE('',*,*,#9858,.T.);
#14395=ORIENTED_EDGE('',*,*,#9853,.T.);
#14396=ORIENTED_EDGE('',*,*,#9859,.F.);
#14397=ORIENTED_EDGE('',*,*,#9860,.F.);
#14398=ORIENTED_EDGE('',*,*,#9861,.T.);
#14399=ORIENTED_EDGE('',*,*,#9857,.T.);
#14400=ORIENTED_EDGE('',*,*,#9862,.F.);
#14401=ORIENTED_EDGE('',*,*,#9863,.F.);
#14402=ORIENTED_EDGE('',*,*,#9864,.T.);
#14403=ORIENTED_EDGE('',*,*,#9860,.T.);
#14404=ORIENTED_EDGE('',*,*,#9865,.F.);
#14405=ORIENTED_EDGE('',*,*,#9866,.F.);
#14406=ORIENTED_EDGE('',*,*,#9867,.T.);
#14407=ORIENTED_EDGE('',*,*,#9863,.T.);
#14408=ORIENTED_EDGE('',*,*,#9868,.F.);
#14409=ORIENTED_EDGE('',*,*,#9869,.F.);
#14410=ORIENTED_EDGE('',*,*,#9870,.T.);
#14411=ORIENTED_EDGE('',*,*,#9866,.T.);
#14412=ORIENTED_EDGE('',*,*,#9871,.F.);
#14413=ORIENTED_EDGE('',*,*,#9855,.T.);
#14414=ORIENTED_EDGE('',*,*,#9872,.T.);
#14415=ORIENTED_EDGE('',*,*,#9873,.F.);
#14416=ORIENTED_EDGE('',*,*,#9874,.F.);
#14417=ORIENTED_EDGE('',*,*,#9875,.T.);
#14418=ORIENTED_EDGE('',*,*,#9875,.F.);
#14419=ORIENTED_EDGE('',*,*,#9876,.F.);
#14420=ORIENTED_EDGE('',*,*,#9852,.F.);
#14421=ORIENTED_EDGE('',*,*,#9849,.F.);
#14422=ORIENTED_EDGE('',*,*,#9846,.F.);
#14423=ORIENTED_EDGE('',*,*,#9843,.F.);
#14424=ORIENTED_EDGE('',*,*,#9840,.F.);
#14425=ORIENTED_EDGE('',*,*,#9837,.F.);
#14426=ORIENTED_EDGE('',*,*,#9877,.F.);
#14427=ORIENTED_EDGE('',*,*,#9878,.T.);
#14428=ORIENTED_EDGE('',*,*,#9871,.T.);
#14429=ORIENTED_EDGE('',*,*,#9868,.T.);
#14430=ORIENTED_EDGE('',*,*,#9865,.T.);
#14431=ORIENTED_EDGE('',*,*,#9862,.T.);
#14432=ORIENTED_EDGE('',*,*,#9859,.T.);
#14433=ORIENTED_EDGE('',*,*,#9856,.T.);
#14434=ORIENTED_EDGE('',*,*,#9869,.T.);
#14435=ORIENTED_EDGE('',*,*,#9878,.F.);
#14436=ORIENTED_EDGE('',*,*,#9879,.F.);
#14437=ORIENTED_EDGE('',*,*,#9880,.T.);
#14438=ORIENTED_EDGE('',*,*,#9872,.F.);
#14439=ORIENTED_EDGE('',*,*,#9854,.F.);
#14440=ORIENTED_EDGE('',*,*,#9858,.F.);
#14441=ORIENTED_EDGE('',*,*,#9861,.F.);
#14442=ORIENTED_EDGE('',*,*,#9864,.F.);
#14443=ORIENTED_EDGE('',*,*,#9867,.F.);
#14444=ORIENTED_EDGE('',*,*,#9870,.F.);
#14445=ORIENTED_EDGE('',*,*,#9880,.F.);
#14446=ORIENTED_EDGE('',*,*,#9881,.F.);
#14447=ORIENTED_EDGE('',*,*,#9835,.F.);
#14448=ORIENTED_EDGE('',*,*,#9839,.F.);
#14449=ORIENTED_EDGE('',*,*,#9842,.F.);
#14450=ORIENTED_EDGE('',*,*,#9845,.F.);
#14451=ORIENTED_EDGE('',*,*,#9848,.F.);
#14452=ORIENTED_EDGE('',*,*,#9851,.F.);
#14453=ORIENTED_EDGE('',*,*,#9882,.F.);
#14454=ORIENTED_EDGE('',*,*,#9850,.T.);
#14455=ORIENTED_EDGE('',*,*,#9876,.T.);
#14456=ORIENTED_EDGE('',*,*,#9883,.F.);
#14457=ORIENTED_EDGE('',*,*,#9882,.T.);
#14458=ORIENTED_EDGE('',*,*,#9884,.F.);
#14459=ORIENTED_EDGE('',*,*,#9885,.F.);
#14460=ORIENTED_EDGE('',*,*,#9886,.T.);
#14461=ORIENTED_EDGE('',*,*,#9884,.T.);
#14462=ORIENTED_EDGE('',*,*,#9886,.F.);
#14463=ORIENTED_EDGE('',*,*,#9887,.F.);
#14464=ORIENTED_EDGE('',*,*,#9888,.T.);
#14465=ORIENTED_EDGE('',*,*,#9885,.T.);
#14466=ORIENTED_EDGE('',*,*,#9888,.F.);
#14467=ORIENTED_EDGE('',*,*,#9887,.T.);
#14468=ORIENTED_EDGE('',*,*,#9881,.T.);
#14469=ORIENTED_EDGE('',*,*,#9879,.T.);
#14470=ORIENTED_EDGE('',*,*,#9877,.T.);
#14471=ORIENTED_EDGE('',*,*,#9836,.F.);
#14472=ORIENTED_EDGE('',*,*,#9889,.F.);
#14473=ORIENTED_EDGE('',*,*,#9890,.T.);
#14474=ORIENTED_EDGE('',*,*,#9873,.T.);
#14475=ORIENTED_EDGE('',*,*,#9883,.T.);
#14476=ORIENTED_EDGE('',*,*,#9874,.T.);
#14477=ORIENTED_EDGE('',*,*,#9890,.F.);
#14478=ORIENTED_EDGE('',*,*,#9889,.T.);
#14479=ORIENTED_EDGE('',*,*,#9891,.T.);
#14480=ORIENTED_EDGE('',*,*,#9892,.T.);
#14481=ORIENTED_EDGE('',*,*,#9893,.T.);
#14482=ORIENTED_EDGE('',*,*,#9894,.T.);
#14483=ORIENTED_EDGE('',*,*,#9895,.T.);
#14484=ORIENTED_EDGE('',*,*,#9893,.F.);
#14485=ORIENTED_EDGE('',*,*,#9894,.F.);
#14486=ORIENTED_EDGE('',*,*,#9895,.F.);
#14487=ORIENTED_EDGE('',*,*,#9896,.T.);
#14488=ORIENTED_EDGE('',*,*,#9897,.T.);
#14489=ORIENTED_EDGE('',*,*,#9896,.F.);
#14490=ORIENTED_EDGE('',*,*,#9898,.F.);
#14491=ORIENTED_EDGE('',*,*,#9899,.T.);
#14492=ORIENTED_EDGE('',*,*,#9891,.F.);
#14493=ORIENTED_EDGE('',*,*,#9892,.F.);
#14494=ORIENTED_EDGE('',*,*,#9899,.F.);
#14495=ORIENTED_EDGE('',*,*,#9900,.T.);
#14496=ORIENTED_EDGE('',*,*,#9901,.F.);
#14497=ORIENTED_EDGE('',*,*,#9900,.F.);
#14498=ORIENTED_EDGE('',*,*,#9902,.T.);
#14499=ORIENTED_EDGE('',*,*,#9903,.F.);
#14500=ORIENTED_EDGE('',*,*,#9902,.F.);
#14501=ORIENTED_EDGE('',*,*,#9901,.T.);
#14502=ORIENTED_EDGE('',*,*,#9904,.T.);
#14503=ORIENTED_EDGE('',*,*,#9905,.F.);
#14504=ORIENTED_EDGE('',*,*,#9904,.F.);
#14505=ORIENTED_EDGE('',*,*,#9905,.T.);
#14506=ORIENTED_EDGE('',*,*,#9906,.T.);
#14507=ORIENTED_EDGE('',*,*,#9907,.T.);
#14508=ORIENTED_EDGE('',*,*,#9908,.F.);
#14509=ORIENTED_EDGE('',*,*,#9907,.F.);
#14510=ORIENTED_EDGE('',*,*,#9909,.F.);
#14511=ORIENTED_EDGE('',*,*,#9908,.T.);
#14512=ORIENTED_EDGE('',*,*,#9897,.F.);
#14513=ORIENTED_EDGE('',*,*,#9910,.T.);
#14514=ORIENTED_EDGE('',*,*,#9909,.T.);
#14515=ORIENTED_EDGE('',*,*,#9910,.F.);
#14516=ORIENTED_EDGE('',*,*,#9898,.T.);
#14517=ORIENTED_EDGE('',*,*,#9903,.T.);
#14518=ORIENTED_EDGE('',*,*,#9906,.F.);
#14519=ORIENTED_EDGE('',*,*,#9911,.T.);
#14520=ORIENTED_EDGE('',*,*,#9912,.T.);
#14521=ORIENTED_EDGE('',*,*,#9913,.F.);
#14522=ORIENTED_EDGE('',*,*,#9912,.F.);
#14523=ORIENTED_EDGE('',*,*,#9914,.F.);
#14524=ORIENTED_EDGE('',*,*,#9913,.T.);
#14525=ORIENTED_EDGE('',*,*,#9915,.F.);
#14526=ORIENTED_EDGE('',*,*,#9916,.T.);
#14527=ORIENTED_EDGE('',*,*,#9914,.T.);
#14528=ORIENTED_EDGE('',*,*,#9916,.F.);
#14529=ORIENTED_EDGE('',*,*,#9915,.T.);
#14530=ORIENTED_EDGE('',*,*,#9911,.F.);
#14531=ORIENTED_EDGE('',*,*,#9917,.T.);
#14532=ORIENTED_EDGE('',*,*,#9918,.T.);
#14533=ORIENTED_EDGE('',*,*,#9919,.T.);
#14534=ORIENTED_EDGE('',*,*,#9920,.T.);
#14535=ORIENTED_EDGE('',*,*,#9918,.F.);
#14536=ORIENTED_EDGE('',*,*,#9919,.F.);
#14537=ORIENTED_EDGE('',*,*,#9920,.F.);
#14538=ORIENTED_EDGE('',*,*,#9921,.T.);
#14539=ORIENTED_EDGE('',*,*,#9922,.T.);
#14540=ORIENTED_EDGE('',*,*,#9921,.F.);
#14541=ORIENTED_EDGE('',*,*,#9917,.F.);
#14542=ORIENTED_EDGE('',*,*,#9923,.F.);
#14543=ORIENTED_EDGE('',*,*,#9923,.T.);
#14544=ORIENTED_EDGE('',*,*,#9924,.T.);
#14545=ORIENTED_EDGE('',*,*,#9925,.F.);
#14546=ORIENTED_EDGE('',*,*,#9924,.F.);
#14547=ORIENTED_EDGE('',*,*,#9926,.F.);
#14548=ORIENTED_EDGE('',*,*,#9925,.T.);
#14549=ORIENTED_EDGE('',*,*,#9922,.F.);
#14550=ORIENTED_EDGE('',*,*,#9927,.T.);
#14551=ORIENTED_EDGE('',*,*,#9926,.T.);
#14552=ORIENTED_EDGE('',*,*,#9927,.F.);
#14553=ORIENTED_EDGE('',*,*,#9928,.T.);
#14554=ORIENTED_EDGE('',*,*,#9929,.T.);
#14555=ORIENTED_EDGE('',*,*,#9930,.T.);
#14556=ORIENTED_EDGE('',*,*,#9929,.F.);
#14557=ORIENTED_EDGE('',*,*,#9930,.F.);
#14558=ORIENTED_EDGE('',*,*,#9931,.T.);
#14559=ORIENTED_EDGE('',*,*,#9932,.F.);
#14560=ORIENTED_EDGE('',*,*,#9931,.F.);
#14561=ORIENTED_EDGE('',*,*,#9933,.T.);
#14562=ORIENTED_EDGE('',*,*,#9928,.F.);
#14563=ORIENTED_EDGE('',*,*,#9934,.T.);
#14564=ORIENTED_EDGE('',*,*,#9935,.T.);
#14565=ORIENTED_EDGE('',*,*,#9932,.T.);
#14566=ORIENTED_EDGE('',*,*,#9935,.F.);
#14567=ORIENTED_EDGE('',*,*,#9936,.F.);
#14568=ORIENTED_EDGE('',*,*,#9934,.F.);
#14569=ORIENTED_EDGE('',*,*,#9936,.T.);
#14570=ORIENTED_EDGE('',*,*,#9937,.T.);
#14571=ORIENTED_EDGE('',*,*,#9938,.T.);
#14572=ORIENTED_EDGE('',*,*,#9939,.T.);
#14573=ORIENTED_EDGE('',*,*,#9940,.T.);
#14574=ORIENTED_EDGE('',*,*,#9941,.T.);
#14575=ORIENTED_EDGE('',*,*,#9942,.T.);
#14576=ORIENTED_EDGE('',*,*,#9943,.T.);
#14577=ORIENTED_EDGE('',*,*,#9944,.T.);
#14578=ORIENTED_EDGE('',*,*,#9945,.T.);
#14579=ORIENTED_EDGE('',*,*,#9946,.T.);
#14580=ORIENTED_EDGE('',*,*,#9947,.T.);
#14581=ORIENTED_EDGE('',*,*,#9948,.T.);
#14582=ORIENTED_EDGE('',*,*,#9949,.T.);
#14583=ORIENTED_EDGE('',*,*,#9950,.T.);
#14584=ORIENTED_EDGE('',*,*,#9937,.F.);
#14585=ORIENTED_EDGE('',*,*,#9946,.F.);
#14586=ORIENTED_EDGE('',*,*,#9951,.T.);
#14587=ORIENTED_EDGE('',*,*,#9952,.T.);
#14588=ORIENTED_EDGE('',*,*,#9953,.T.);
#14589=ORIENTED_EDGE('',*,*,#9954,.T.);
#14590=ORIENTED_EDGE('',*,*,#9955,.T.);
#14591=ORIENTED_EDGE('',*,*,#9944,.F.);
#14592=ORIENTED_EDGE('',*,*,#9956,.T.);
#14593=ORIENTED_EDGE('',*,*,#9957,.T.);
#14594=ORIENTED_EDGE('',*,*,#9958,.T.);
#14595=ORIENTED_EDGE('',*,*,#9959,.T.);
#14596=ORIENTED_EDGE('',*,*,#9960,.T.);
#14597=ORIENTED_EDGE('',*,*,#9945,.F.);
#14598=ORIENTED_EDGE('',*,*,#9960,.F.);
#14599=ORIENTED_EDGE('',*,*,#9951,.F.);
#14600=ORIENTED_EDGE('',*,*,#9943,.F.);
#14601=ORIENTED_EDGE('',*,*,#9961,.F.);
#14602=ORIENTED_EDGE('',*,*,#9956,.F.);
#14603=ORIENTED_EDGE('',*,*,#9941,.F.);
#14604=ORIENTED_EDGE('',*,*,#9962,.F.);
#14605=ORIENTED_EDGE('',*,*,#9963,.F.);
#14606=ORIENTED_EDGE('',*,*,#9939,.F.);
#14607=ORIENTED_EDGE('',*,*,#9964,.F.);
#14608=ORIENTED_EDGE('',*,*,#9965,.F.);
#14609=ORIENTED_EDGE('',*,*,#9949,.F.);
#14610=ORIENTED_EDGE('',*,*,#9966,.F.);
#14611=ORIENTED_EDGE('',*,*,#9967,.F.);
#14612=ORIENTED_EDGE('',*,*,#9947,.F.);
#14613=ORIENTED_EDGE('',*,*,#9955,.F.);
#14614=ORIENTED_EDGE('',*,*,#9968,.F.);
#14615=ORIENTED_EDGE('',*,*,#9942,.F.);
#14616=ORIENTED_EDGE('',*,*,#9963,.T.);
#14617=ORIENTED_EDGE('',*,*,#9969,.T.);
#14618=ORIENTED_EDGE('',*,*,#9970,.T.);
#14619=ORIENTED_EDGE('',*,*,#9971,.T.);
#14620=ORIENTED_EDGE('',*,*,#9961,.T.);
#14621=ORIENTED_EDGE('',*,*,#9972,.F.);
#14622=ORIENTED_EDGE('',*,*,#9957,.F.);
#14623=ORIENTED_EDGE('',*,*,#9971,.F.);
#14624=ORIENTED_EDGE('',*,*,#9969,.F.);
#14625=ORIENTED_EDGE('',*,*,#9973,.F.);
#14626=ORIENTED_EDGE('',*,*,#9974,.F.);
#14627=ORIENTED_EDGE('',*,*,#9975,.F.);
#14628=ORIENTED_EDGE('',*,*,#9952,.F.);
#14629=ORIENTED_EDGE('',*,*,#9959,.F.);
#14630=ORIENTED_EDGE('',*,*,#9976,.F.);
#14631=ORIENTED_EDGE('',*,*,#9977,.F.);
#14632=ORIENTED_EDGE('',*,*,#9978,.F.);
#14633=ORIENTED_EDGE('',*,*,#9979,.F.);
#14634=ORIENTED_EDGE('',*,*,#9980,.F.);
#14635=ORIENTED_EDGE('',*,*,#9954,.F.);
#14636=ORIENTED_EDGE('',*,*,#9981,.F.);
#14637=ORIENTED_EDGE('',*,*,#9982,.F.);
#14638=ORIENTED_EDGE('',*,*,#9983,.F.);
#14639=ORIENTED_EDGE('',*,*,#9948,.F.);
#14640=ORIENTED_EDGE('',*,*,#9968,.T.);
#14641=ORIENTED_EDGE('',*,*,#9980,.T.);
#14642=ORIENTED_EDGE('',*,*,#9984,.T.);
#14643=ORIENTED_EDGE('',*,*,#9982,.T.);
#14644=ORIENTED_EDGE('',*,*,#9966,.T.);
#14645=ORIENTED_EDGE('',*,*,#9985,.T.);
#14646=ORIENTED_EDGE('',*,*,#9986,.T.);
#14647=ORIENTED_EDGE('',*,*,#9983,.T.);
#14648=ORIENTED_EDGE('',*,*,#9987,.T.);
#14649=ORIENTED_EDGE('',*,*,#9950,.F.);
#14650=ORIENTED_EDGE('',*,*,#9967,.T.);
#14651=ORIENTED_EDGE('',*,*,#9981,.T.);
#14652=ORIENTED_EDGE('',*,*,#9988,.T.);
#14653=ORIENTED_EDGE('',*,*,#9977,.T.);
#14654=ORIENTED_EDGE('',*,*,#9964,.T.);
#14655=ORIENTED_EDGE('',*,*,#9938,.F.);
#14656=ORIENTED_EDGE('',*,*,#9989,.T.);
#14657=ORIENTED_EDGE('',*,*,#9990,.T.);
#14658=ORIENTED_EDGE('',*,*,#9979,.T.);
#14659=ORIENTED_EDGE('',*,*,#9991,.T.);
#14660=ORIENTED_EDGE('',*,*,#9992,.T.);
#14661=ORIENTED_EDGE('',*,*,#9993,.T.);
#14662=ORIENTED_EDGE('',*,*,#9978,.T.);
#14663=ORIENTED_EDGE('',*,*,#9994,.T.);
#14664=ORIENTED_EDGE('',*,*,#9940,.F.);
#14665=ORIENTED_EDGE('',*,*,#9965,.T.);
#14666=ORIENTED_EDGE('',*,*,#9976,.T.);
#14667=ORIENTED_EDGE('',*,*,#9995,.T.);
#14668=ORIENTED_EDGE('',*,*,#9973,.T.);
#14669=ORIENTED_EDGE('',*,*,#9962,.T.);
#14670=ORIENTED_EDGE('',*,*,#9996,.T.);
#14671=ORIENTED_EDGE('',*,*,#9997,.T.);
#14672=ORIENTED_EDGE('',*,*,#9975,.T.);
#14673=ORIENTED_EDGE('',*,*,#9998,.T.);
#14674=ORIENTED_EDGE('',*,*,#9999,.T.);
#14675=ORIENTED_EDGE('',*,*,#10000,.T.);
#14676=ORIENTED_EDGE('',*,*,#9974,.T.);
#14677=ORIENTED_EDGE('',*,*,#10001,.T.);
#14678=ORIENTED_EDGE('',*,*,#10002,.T.);
#14679=ORIENTED_EDGE('',*,*,#10003,.T.);
#14680=ORIENTED_EDGE('',*,*,#9972,.T.);
#14681=ORIENTED_EDGE('',*,*,#10004,.T.);
#14682=ORIENTED_EDGE('',*,*,#9991,.F.);
#14683=ORIENTED_EDGE('',*,*,#9953,.F.);
#14684=ORIENTED_EDGE('',*,*,#9997,.F.);
#14685=ORIENTED_EDGE('',*,*,#10005,.T.);
#14686=ORIENTED_EDGE('',*,*,#9998,.F.);
#14687=ORIENTED_EDGE('',*,*,#9958,.F.);
#14688=ORIENTED_EDGE('',*,*,#10003,.F.);
#14689=ORIENTED_EDGE('',*,*,#10006,.T.);
#14690=ORIENTED_EDGE('',*,*,#10004,.F.);
#14691=ORIENTED_EDGE('',*,*,#9970,.F.);
#14692=ORIENTED_EDGE('',*,*,#10000,.F.);
#14693=ORIENTED_EDGE('',*,*,#10007,.T.);
#14694=ORIENTED_EDGE('',*,*,#9933,.F.);
#14695=ORIENTED_EDGE('',*,*,#10008,.T.);
#14696=ORIENTED_EDGE('',*,*,#10009,.F.);
#14697=ORIENTED_EDGE('',*,*,#9985,.F.);
#14698=ORIENTED_EDGE('',*,*,#10010,.F.);
#14699=ORIENTED_EDGE('',*,*,#9989,.F.);
#14700=ORIENTED_EDGE('',*,*,#10005,.F.);
#14701=ORIENTED_EDGE('',*,*,#9996,.F.);
#14702=ORIENTED_EDGE('',*,*,#10006,.F.);
#14703=ORIENTED_EDGE('',*,*,#10002,.F.);
#14704=ORIENTED_EDGE('',*,*,#10007,.F.);
#14705=ORIENTED_EDGE('',*,*,#9999,.F.);
#14706=ORIENTED_EDGE('',*,*,#10011,.F.);
#14707=ORIENTED_EDGE('',*,*,#9992,.F.);
#14708=ORIENTED_EDGE('',*,*,#10012,.F.);
#14709=ORIENTED_EDGE('',*,*,#10008,.F.);
#14710=ORIENTED_EDGE('',*,*,#9993,.F.);
#14711=ORIENTED_EDGE('',*,*,#10011,.T.);
#14712=ORIENTED_EDGE('',*,*,#10001,.F.);
#14713=ORIENTED_EDGE('',*,*,#9995,.F.);
#14714=ORIENTED_EDGE('',*,*,#9986,.F.);
#14715=ORIENTED_EDGE('',*,*,#10009,.T.);
#14716=ORIENTED_EDGE('',*,*,#10012,.T.);
#14717=ORIENTED_EDGE('',*,*,#9994,.F.);
#14718=ORIENTED_EDGE('',*,*,#9988,.F.);
#14719=ORIENTED_EDGE('',*,*,#9990,.F.);
#14720=ORIENTED_EDGE('',*,*,#10010,.T.);
#14721=ORIENTED_EDGE('',*,*,#9987,.F.);
#14722=ORIENTED_EDGE('',*,*,#9984,.F.);
#14723=ORIENTED_EDGE('',*,*,#10013,.T.);
#14724=ORIENTED_EDGE('',*,*,#10013,.F.);
#14725=ORIENTED_EDGE('',*,*,#10014,.T.);
#14726=ORIENTED_EDGE('',*,*,#10015,.T.);
#14727=ORIENTED_EDGE('',*,*,#10016,.F.);
#14728=ORIENTED_EDGE('',*,*,#10015,.F.);
#14729=ORIENTED_EDGE('',*,*,#10016,.T.);
#14730=ORIENTED_EDGE('',*,*,#10014,.F.);
#14731=ORIENTED_EDGE('',*,*,#10017,.F.);
#14732=ORIENTED_EDGE('',*,*,#10018,.T.);
#14733=ORIENTED_EDGE('',*,*,#10019,.T.);
#14734=ORIENTED_EDGE('',*,*,#10020,.T.);
#14735=ORIENTED_EDGE('',*,*,#10021,.F.);
#14736=ORIENTED_EDGE('',*,*,#10022,.T.);
#14737=ORIENTED_EDGE('',*,*,#10017,.T.);
#14738=ORIENTED_EDGE('',*,*,#10023,.T.);
#14739=ORIENTED_EDGE('',*,*,#10024,.F.);
#14740=ORIENTED_EDGE('',*,*,#10025,.T.);
#14741=ORIENTED_EDGE('',*,*,#10021,.T.);
#14742=ORIENTED_EDGE('',*,*,#10026,.T.);
#14743=ORIENTED_EDGE('',*,*,#10027,.F.);
#14744=ORIENTED_EDGE('',*,*,#10028,.T.);
#14745=ORIENTED_EDGE('',*,*,#10024,.T.);
#14746=ORIENTED_EDGE('',*,*,#10029,.T.);
#14747=ORIENTED_EDGE('',*,*,#10030,.F.);
#14748=ORIENTED_EDGE('',*,*,#10031,.T.);
#14749=ORIENTED_EDGE('',*,*,#10032,.F.);
#14750=ORIENTED_EDGE('',*,*,#10033,.F.);
#14751=ORIENTED_EDGE('',*,*,#10034,.F.);
#14752=ORIENTED_EDGE('',*,*,#10035,.T.);
#14753=ORIENTED_EDGE('',*,*,#10030,.T.);
#14754=ORIENTED_EDGE('',*,*,#10036,.F.);
#14755=ORIENTED_EDGE('',*,*,#10037,.F.);
#14756=ORIENTED_EDGE('',*,*,#10038,.T.);
#14757=ORIENTED_EDGE('',*,*,#10034,.T.);
#14758=ORIENTED_EDGE('',*,*,#10039,.F.);
#14759=ORIENTED_EDGE('',*,*,#10040,.F.);
#14760=ORIENTED_EDGE('',*,*,#10041,.T.);
#14761=ORIENTED_EDGE('',*,*,#10037,.T.);
#14762=ORIENTED_EDGE('',*,*,#10042,.F.);
#14763=ORIENTED_EDGE('',*,*,#10032,.T.);
#14764=ORIENTED_EDGE('',*,*,#10043,.T.);
#14765=ORIENTED_EDGE('',*,*,#10044,.F.);
#14766=ORIENTED_EDGE('',*,*,#10045,.F.);
#14767=ORIENTED_EDGE('',*,*,#10046,.T.);
#14768=ORIENTED_EDGE('',*,*,#10046,.F.);
#14769=ORIENTED_EDGE('',*,*,#10047,.F.);
#14770=ORIENTED_EDGE('',*,*,#10029,.F.);
#14771=ORIENTED_EDGE('',*,*,#10026,.F.);
#14772=ORIENTED_EDGE('',*,*,#10023,.F.);
#14773=ORIENTED_EDGE('',*,*,#10020,.F.);
#14774=ORIENTED_EDGE('',*,*,#10048,.F.);
#14775=ORIENTED_EDGE('',*,*,#10049,.T.);
#14776=ORIENTED_EDGE('',*,*,#10042,.T.);
#14777=ORIENTED_EDGE('',*,*,#10039,.T.);
#14778=ORIENTED_EDGE('',*,*,#10036,.T.);
#14779=ORIENTED_EDGE('',*,*,#10033,.T.);
#14780=ORIENTED_EDGE('',*,*,#10050,.T.);
#14781=ORIENTED_EDGE('',*,*,#10051,.T.);
#14782=ORIENTED_EDGE('',*,*,#10052,.T.);
#14783=ORIENTED_EDGE('',*,*,#10053,.T.);
#14784=ORIENTED_EDGE('',*,*,#10048,.T.);
#14785=ORIENTED_EDGE('',*,*,#10040,.T.);
#14786=ORIENTED_EDGE('',*,*,#10049,.F.);
#14787=ORIENTED_EDGE('',*,*,#10053,.F.);
#14788=ORIENTED_EDGE('',*,*,#10054,.T.);
#14789=ORIENTED_EDGE('',*,*,#10043,.F.);
#14790=ORIENTED_EDGE('',*,*,#10031,.F.);
#14791=ORIENTED_EDGE('',*,*,#10035,.F.);
#14792=ORIENTED_EDGE('',*,*,#10038,.F.);
#14793=ORIENTED_EDGE('',*,*,#10041,.F.);
#14794=ORIENTED_EDGE('',*,*,#10054,.F.);
#14795=ORIENTED_EDGE('',*,*,#10052,.F.);
#14796=ORIENTED_EDGE('',*,*,#10018,.F.);
#14797=ORIENTED_EDGE('',*,*,#10022,.F.);
#14798=ORIENTED_EDGE('',*,*,#10025,.F.);
#14799=ORIENTED_EDGE('',*,*,#10028,.F.);
#14800=ORIENTED_EDGE('',*,*,#10055,.F.);
#14801=ORIENTED_EDGE('',*,*,#10056,.F.);
#14802=ORIENTED_EDGE('',*,*,#10057,.T.);
#14803=ORIENTED_EDGE('',*,*,#10058,.T.);
#14804=ORIENTED_EDGE('',*,*,#10059,.F.);
#14805=ORIENTED_EDGE('',*,*,#10060,.F.);
#14806=ORIENTED_EDGE('',*,*,#10061,.T.);
#14807=ORIENTED_EDGE('',*,*,#10062,.T.);
#14808=ORIENTED_EDGE('',*,*,#10057,.F.);
#14809=ORIENTED_EDGE('',*,*,#10063,.F.);
#14810=ORIENTED_EDGE('',*,*,#10064,.T.);
#14811=ORIENTED_EDGE('',*,*,#10065,.T.);
#14812=ORIENTED_EDGE('',*,*,#10061,.F.);
#14813=ORIENTED_EDGE('',*,*,#10066,.F.);
#14814=ORIENTED_EDGE('',*,*,#10067,.T.);
#14815=ORIENTED_EDGE('',*,*,#10068,.T.);
#14816=ORIENTED_EDGE('',*,*,#10064,.F.);
#14817=ORIENTED_EDGE('',*,*,#10069,.F.);
#14818=ORIENTED_EDGE('',*,*,#10070,.T.);
#14819=ORIENTED_EDGE('',*,*,#10071,.T.);
#14820=ORIENTED_EDGE('',*,*,#10067,.F.);
#14821=ORIENTED_EDGE('',*,*,#10072,.F.);
#14822=ORIENTED_EDGE('',*,*,#10059,.T.);
#14823=ORIENTED_EDGE('',*,*,#10073,.T.);
#14824=ORIENTED_EDGE('',*,*,#10070,.F.);
#14825=ORIENTED_EDGE('',*,*,#10073,.F.);
#14826=ORIENTED_EDGE('',*,*,#10058,.F.);
#14827=ORIENTED_EDGE('',*,*,#10062,.F.);
#14828=ORIENTED_EDGE('',*,*,#10065,.F.);
#14829=ORIENTED_EDGE('',*,*,#10068,.F.);
#14830=ORIENTED_EDGE('',*,*,#10071,.F.);
#14831=ORIENTED_EDGE('',*,*,#10074,.F.);
#14832=ORIENTED_EDGE('',*,*,#10050,.F.);
#14833=ORIENTED_EDGE('',*,*,#10019,.F.);
#14834=ORIENTED_EDGE('',*,*,#10051,.F.);
#14835=ORIENTED_EDGE('',*,*,#10075,.T.);
#14836=ORIENTED_EDGE('',*,*,#10074,.T.);
#14837=ORIENTED_EDGE('',*,*,#10075,.F.);
#14838=ORIENTED_EDGE('',*,*,#10027,.T.);
#14839=ORIENTED_EDGE('',*,*,#10047,.T.);
#14840=ORIENTED_EDGE('',*,*,#10076,.F.);
#14841=ORIENTED_EDGE('',*,*,#10055,.T.);
#14842=ORIENTED_EDGE('',*,*,#10077,.F.);
#14843=ORIENTED_EDGE('',*,*,#10078,.T.);
#14844=ORIENTED_EDGE('',*,*,#10044,.T.);
#14845=ORIENTED_EDGE('',*,*,#10076,.T.);
#14846=ORIENTED_EDGE('',*,*,#10045,.T.);
#14847=ORIENTED_EDGE('',*,*,#10078,.F.);
#14848=ORIENTED_EDGE('',*,*,#10077,.T.);
#14849=ORIENTED_EDGE('',*,*,#10056,.T.);
#14850=ORIENTED_EDGE('',*,*,#10072,.T.);
#14851=ORIENTED_EDGE('',*,*,#10069,.T.);
#14852=ORIENTED_EDGE('',*,*,#10066,.T.);
#14853=ORIENTED_EDGE('',*,*,#10063,.T.);
#14854=ORIENTED_EDGE('',*,*,#10060,.T.);
#14855=ORIENTED_EDGE('',*,*,#10079,.F.);
#14856=ORIENTED_EDGE('',*,*,#10080,.T.);
#14857=ORIENTED_EDGE('',*,*,#10081,.T.);
#14858=ORIENTED_EDGE('',*,*,#10082,.T.);
#14859=ORIENTED_EDGE('',*,*,#10083,.F.);
#14860=ORIENTED_EDGE('',*,*,#10084,.T.);
#14861=ORIENTED_EDGE('',*,*,#10079,.T.);
#14862=ORIENTED_EDGE('',*,*,#10085,.T.);
#14863=ORIENTED_EDGE('',*,*,#10086,.F.);
#14864=ORIENTED_EDGE('',*,*,#10087,.T.);
#14865=ORIENTED_EDGE('',*,*,#10083,.T.);
#14866=ORIENTED_EDGE('',*,*,#10088,.T.);
#14867=ORIENTED_EDGE('',*,*,#10089,.F.);
#14868=ORIENTED_EDGE('',*,*,#10090,.T.);
#14869=ORIENTED_EDGE('',*,*,#10086,.T.);
#14870=ORIENTED_EDGE('',*,*,#10091,.T.);
#14871=ORIENTED_EDGE('',*,*,#10092,.F.);
#14872=ORIENTED_EDGE('',*,*,#10093,.T.);
#14873=ORIENTED_EDGE('',*,*,#10089,.T.);
#14874=ORIENTED_EDGE('',*,*,#10094,.T.);
#14875=ORIENTED_EDGE('',*,*,#10095,.F.);
#14876=ORIENTED_EDGE('',*,*,#10096,.T.);
#14877=ORIENTED_EDGE('',*,*,#10092,.T.);
#14878=ORIENTED_EDGE('',*,*,#10097,.T.);
#14879=ORIENTED_EDGE('',*,*,#10098,.F.);
#14880=ORIENTED_EDGE('',*,*,#10099,.T.);
#14881=ORIENTED_EDGE('',*,*,#10095,.T.);
#14882=ORIENTED_EDGE('',*,*,#10100,.T.);
#14883=ORIENTED_EDGE('',*,*,#10101,.F.);
#14884=ORIENTED_EDGE('',*,*,#10102,.T.);
#14885=ORIENTED_EDGE('',*,*,#10098,.T.);
#14886=ORIENTED_EDGE('',*,*,#10103,.T.);
#14887=ORIENTED_EDGE('',*,*,#10104,.F.);
#14888=ORIENTED_EDGE('',*,*,#10105,.T.);
#14889=ORIENTED_EDGE('',*,*,#10101,.T.);
#14890=ORIENTED_EDGE('',*,*,#10106,.T.);
#14891=ORIENTED_EDGE('',*,*,#10107,.F.);
#14892=ORIENTED_EDGE('',*,*,#10108,.T.);
#14893=ORIENTED_EDGE('',*,*,#10104,.T.);
#14894=ORIENTED_EDGE('',*,*,#10109,.T.);
#14895=ORIENTED_EDGE('',*,*,#10110,.F.);
#14896=ORIENTED_EDGE('',*,*,#10111,.T.);
#14897=ORIENTED_EDGE('',*,*,#10107,.T.);
#14898=ORIENTED_EDGE('',*,*,#10112,.T.);
#14899=ORIENTED_EDGE('',*,*,#10113,.F.);
#14900=ORIENTED_EDGE('',*,*,#10114,.T.);
#14901=ORIENTED_EDGE('',*,*,#10110,.T.);
#14902=ORIENTED_EDGE('',*,*,#10115,.T.);
#14903=ORIENTED_EDGE('',*,*,#10116,.F.);
#14904=ORIENTED_EDGE('',*,*,#10117,.T.);
#14905=ORIENTED_EDGE('',*,*,#10113,.T.);
#14906=ORIENTED_EDGE('',*,*,#10118,.T.);
#14907=ORIENTED_EDGE('',*,*,#10119,.F.);
#14908=ORIENTED_EDGE('',*,*,#10120,.T.);
#14909=ORIENTED_EDGE('',*,*,#10116,.T.);
#14910=ORIENTED_EDGE('',*,*,#10121,.T.);
#14911=ORIENTED_EDGE('',*,*,#10122,.F.);
#14912=ORIENTED_EDGE('',*,*,#10123,.T.);
#14913=ORIENTED_EDGE('',*,*,#10119,.T.);
#14914=ORIENTED_EDGE('',*,*,#10124,.T.);
#14915=ORIENTED_EDGE('',*,*,#10125,.F.);
#14916=ORIENTED_EDGE('',*,*,#10126,.T.);
#14917=ORIENTED_EDGE('',*,*,#10127,.F.);
#14918=ORIENTED_EDGE('',*,*,#10128,.F.);
#14919=ORIENTED_EDGE('',*,*,#10129,.F.);
#14920=ORIENTED_EDGE('',*,*,#10130,.T.);
#14921=ORIENTED_EDGE('',*,*,#10125,.T.);
#14922=ORIENTED_EDGE('',*,*,#10131,.F.);
#14923=ORIENTED_EDGE('',*,*,#10132,.F.);
#14924=ORIENTED_EDGE('',*,*,#10133,.T.);
#14925=ORIENTED_EDGE('',*,*,#10129,.T.);
#14926=ORIENTED_EDGE('',*,*,#10134,.F.);
#14927=ORIENTED_EDGE('',*,*,#10135,.F.);
#14928=ORIENTED_EDGE('',*,*,#10136,.T.);
#14929=ORIENTED_EDGE('',*,*,#10132,.T.);
#14930=ORIENTED_EDGE('',*,*,#10137,.F.);
#14931=ORIENTED_EDGE('',*,*,#10138,.F.);
#14932=ORIENTED_EDGE('',*,*,#10139,.T.);
#14933=ORIENTED_EDGE('',*,*,#10135,.T.);
#14934=ORIENTED_EDGE('',*,*,#10140,.F.);
#14935=ORIENTED_EDGE('',*,*,#10141,.F.);
#14936=ORIENTED_EDGE('',*,*,#10142,.T.);
#14937=ORIENTED_EDGE('',*,*,#10138,.T.);
#14938=ORIENTED_EDGE('',*,*,#10143,.F.);
#14939=ORIENTED_EDGE('',*,*,#10144,.F.);
#14940=ORIENTED_EDGE('',*,*,#10145,.T.);
#14941=ORIENTED_EDGE('',*,*,#10141,.T.);
#14942=ORIENTED_EDGE('',*,*,#10146,.F.);
#14943=ORIENTED_EDGE('',*,*,#10147,.F.);
#14944=ORIENTED_EDGE('',*,*,#10148,.T.);
#14945=ORIENTED_EDGE('',*,*,#10144,.T.);
#14946=ORIENTED_EDGE('',*,*,#10149,.F.);
#14947=ORIENTED_EDGE('',*,*,#10150,.F.);
#14948=ORIENTED_EDGE('',*,*,#10151,.T.);
#14949=ORIENTED_EDGE('',*,*,#10147,.T.);
#14950=ORIENTED_EDGE('',*,*,#10152,.F.);
#14951=ORIENTED_EDGE('',*,*,#10153,.F.);
#14952=ORIENTED_EDGE('',*,*,#10154,.T.);
#14953=ORIENTED_EDGE('',*,*,#10150,.T.);
#14954=ORIENTED_EDGE('',*,*,#10155,.F.);
#14955=ORIENTED_EDGE('',*,*,#10156,.F.);
#14956=ORIENTED_EDGE('',*,*,#10157,.T.);
#14957=ORIENTED_EDGE('',*,*,#10153,.T.);
#14958=ORIENTED_EDGE('',*,*,#10158,.F.);
#14959=ORIENTED_EDGE('',*,*,#10159,.F.);
#14960=ORIENTED_EDGE('',*,*,#10160,.T.);
#14961=ORIENTED_EDGE('',*,*,#10156,.T.);
#14962=ORIENTED_EDGE('',*,*,#10161,.F.);
#14963=ORIENTED_EDGE('',*,*,#10162,.F.);
#14964=ORIENTED_EDGE('',*,*,#10163,.T.);
#14965=ORIENTED_EDGE('',*,*,#10159,.T.);
#14966=ORIENTED_EDGE('',*,*,#10164,.F.);
#14967=ORIENTED_EDGE('',*,*,#10165,.F.);
#14968=ORIENTED_EDGE('',*,*,#10166,.T.);
#14969=ORIENTED_EDGE('',*,*,#10162,.T.);
#14970=ORIENTED_EDGE('',*,*,#10167,.F.);
#14971=ORIENTED_EDGE('',*,*,#10168,.F.);
#14972=ORIENTED_EDGE('',*,*,#10169,.F.);
#14973=ORIENTED_EDGE('',*,*,#10124,.F.);
#14974=ORIENTED_EDGE('',*,*,#10121,.F.);
#14975=ORIENTED_EDGE('',*,*,#10118,.F.);
#14976=ORIENTED_EDGE('',*,*,#10115,.F.);
#14977=ORIENTED_EDGE('',*,*,#10112,.F.);
#14978=ORIENTED_EDGE('',*,*,#10109,.F.);
#14979=ORIENTED_EDGE('',*,*,#10106,.F.);
#14980=ORIENTED_EDGE('',*,*,#10103,.F.);
#14981=ORIENTED_EDGE('',*,*,#10100,.F.);
#14982=ORIENTED_EDGE('',*,*,#10097,.F.);
#14983=ORIENTED_EDGE('',*,*,#10094,.F.);
#14984=ORIENTED_EDGE('',*,*,#10091,.F.);
#14985=ORIENTED_EDGE('',*,*,#10088,.F.);
#14986=ORIENTED_EDGE('',*,*,#10085,.F.);
#14987=ORIENTED_EDGE('',*,*,#10082,.F.);
#14988=ORIENTED_EDGE('',*,*,#10170,.F.);
#14989=ORIENTED_EDGE('',*,*,#10171,.T.);
#14990=ORIENTED_EDGE('',*,*,#10167,.T.);
#14991=ORIENTED_EDGE('',*,*,#10164,.T.);
#14992=ORIENTED_EDGE('',*,*,#10161,.T.);
#14993=ORIENTED_EDGE('',*,*,#10158,.T.);
#14994=ORIENTED_EDGE('',*,*,#10155,.T.);
#14995=ORIENTED_EDGE('',*,*,#10152,.T.);
#14996=ORIENTED_EDGE('',*,*,#10149,.T.);
#14997=ORIENTED_EDGE('',*,*,#10146,.T.);
#14998=ORIENTED_EDGE('',*,*,#10143,.T.);
#14999=ORIENTED_EDGE('',*,*,#10140,.T.);
#15000=ORIENTED_EDGE('',*,*,#10137,.T.);
#15001=ORIENTED_EDGE('',*,*,#10134,.T.);
#15002=ORIENTED_EDGE('',*,*,#10131,.T.);
#15003=ORIENTED_EDGE('',*,*,#10128,.T.);
#15004=ORIENTED_EDGE('',*,*,#10172,.T.);
#15005=ORIENTED_EDGE('',*,*,#10173,.T.);
#15006=ORIENTED_EDGE('',*,*,#10174,.T.);
#15007=ORIENTED_EDGE('',*,*,#10175,.T.);
#15008=ORIENTED_EDGE('',*,*,#10170,.T.);
#15009=ORIENTED_EDGE('',*,*,#10165,.T.);
#15010=ORIENTED_EDGE('',*,*,#10171,.F.);
#15011=ORIENTED_EDGE('',*,*,#10175,.F.);
#15012=ORIENTED_EDGE('',*,*,#10176,.T.);
#15013=ORIENTED_EDGE('',*,*,#10177,.F.);
#15014=ORIENTED_EDGE('',*,*,#10126,.F.);
#15015=ORIENTED_EDGE('',*,*,#10130,.F.);
#15016=ORIENTED_EDGE('',*,*,#10133,.F.);
#15017=ORIENTED_EDGE('',*,*,#10136,.F.);
#15018=ORIENTED_EDGE('',*,*,#10139,.F.);
#15019=ORIENTED_EDGE('',*,*,#10142,.F.);
#15020=ORIENTED_EDGE('',*,*,#10145,.F.);
#15021=ORIENTED_EDGE('',*,*,#10148,.F.);
#15022=ORIENTED_EDGE('',*,*,#10151,.F.);
#15023=ORIENTED_EDGE('',*,*,#10154,.F.);
#15024=ORIENTED_EDGE('',*,*,#10157,.F.);
#15025=ORIENTED_EDGE('',*,*,#10160,.F.);
#15026=ORIENTED_EDGE('',*,*,#10163,.F.);
#15027=ORIENTED_EDGE('',*,*,#10166,.F.);
#15028=ORIENTED_EDGE('',*,*,#10176,.F.);
#15029=ORIENTED_EDGE('',*,*,#10174,.F.);
#15030=ORIENTED_EDGE('',*,*,#10080,.F.);
#15031=ORIENTED_EDGE('',*,*,#10084,.F.);
#15032=ORIENTED_EDGE('',*,*,#10087,.F.);
#15033=ORIENTED_EDGE('',*,*,#10090,.F.);
#15034=ORIENTED_EDGE('',*,*,#10093,.F.);
#15035=ORIENTED_EDGE('',*,*,#10096,.F.);
#15036=ORIENTED_EDGE('',*,*,#10099,.F.);
#15037=ORIENTED_EDGE('',*,*,#10102,.F.);
#15038=ORIENTED_EDGE('',*,*,#10105,.F.);
#15039=ORIENTED_EDGE('',*,*,#10108,.F.);
#15040=ORIENTED_EDGE('',*,*,#10111,.F.);
#15041=ORIENTED_EDGE('',*,*,#10114,.F.);
#15042=ORIENTED_EDGE('',*,*,#10117,.F.);
#15043=ORIENTED_EDGE('',*,*,#10120,.F.);
#15044=ORIENTED_EDGE('',*,*,#10123,.F.);
#15045=ORIENTED_EDGE('',*,*,#10178,.F.);
#15046=ORIENTED_EDGE('',*,*,#10179,.F.);
#15047=ORIENTED_EDGE('',*,*,#10180,.F.);
#15048=ORIENTED_EDGE('',*,*,#10181,.F.);
#15049=ORIENTED_EDGE('',*,*,#10182,.F.);
#15050=ORIENTED_EDGE('',*,*,#10183,.F.);
#15051=ORIENTED_EDGE('',*,*,#10181,.T.);
#15052=ORIENTED_EDGE('',*,*,#10184,.T.);
#15053=ORIENTED_EDGE('',*,*,#10185,.F.);
#15054=ORIENTED_EDGE('',*,*,#10186,.F.);
#15055=ORIENTED_EDGE('',*,*,#10184,.F.);
#15056=ORIENTED_EDGE('',*,*,#10180,.T.);
#15057=ORIENTED_EDGE('',*,*,#10182,.T.);
#15058=ORIENTED_EDGE('',*,*,#10183,.T.);
#15059=ORIENTED_EDGE('',*,*,#10186,.T.);
#15060=ORIENTED_EDGE('',*,*,#10187,.F.);
#15061=ORIENTED_EDGE('',*,*,#10188,.T.);
#15062=ORIENTED_EDGE('',*,*,#10189,.T.);
#15063=ORIENTED_EDGE('',*,*,#10190,.T.);
#15064=ORIENTED_EDGE('',*,*,#10191,.F.);
#15065=ORIENTED_EDGE('',*,*,#10192,.T.);
#15066=ORIENTED_EDGE('',*,*,#10193,.T.);
#15067=ORIENTED_EDGE('',*,*,#10194,.T.);
#15068=ORIENTED_EDGE('',*,*,#10195,.F.);
#15069=ORIENTED_EDGE('',*,*,#10196,.T.);
#15070=ORIENTED_EDGE('',*,*,#10197,.T.);
#15071=ORIENTED_EDGE('',*,*,#10198,.T.);
#15072=ORIENTED_EDGE('',*,*,#10199,.F.);
#15073=ORIENTED_EDGE('',*,*,#10200,.T.);
#15074=ORIENTED_EDGE('',*,*,#10201,.T.);
#15075=ORIENTED_EDGE('',*,*,#10202,.T.);
#15076=ORIENTED_EDGE('',*,*,#10203,.F.);
#15077=ORIENTED_EDGE('',*,*,#10204,.T.);
#15078=ORIENTED_EDGE('',*,*,#10205,.T.);
#15079=ORIENTED_EDGE('',*,*,#10206,.T.);
#15080=ORIENTED_EDGE('',*,*,#10207,.F.);
#15081=ORIENTED_EDGE('',*,*,#10208,.T.);
#15082=ORIENTED_EDGE('',*,*,#10209,.T.);
#15083=ORIENTED_EDGE('',*,*,#10210,.T.);
#15084=ORIENTED_EDGE('',*,*,#10211,.F.);
#15085=ORIENTED_EDGE('',*,*,#10212,.T.);
#15086=ORIENTED_EDGE('',*,*,#10213,.T.);
#15087=ORIENTED_EDGE('',*,*,#10214,.T.);
#15088=ORIENTED_EDGE('',*,*,#10215,.F.);
#15089=ORIENTED_EDGE('',*,*,#10216,.T.);
#15090=ORIENTED_EDGE('',*,*,#10217,.T.);
#15091=ORIENTED_EDGE('',*,*,#10218,.T.);
#15092=ORIENTED_EDGE('',*,*,#10219,.F.);
#15093=ORIENTED_EDGE('',*,*,#10220,.T.);
#15094=ORIENTED_EDGE('',*,*,#10221,.T.);
#15095=ORIENTED_EDGE('',*,*,#10222,.T.);
#15096=ORIENTED_EDGE('',*,*,#10223,.F.);
#15097=ORIENTED_EDGE('',*,*,#10224,.T.);
#15098=ORIENTED_EDGE('',*,*,#10225,.T.);
#15099=ORIENTED_EDGE('',*,*,#10226,.T.);
#15100=ORIENTED_EDGE('',*,*,#10227,.F.);
#15101=ORIENTED_EDGE('',*,*,#10228,.T.);
#15102=ORIENTED_EDGE('',*,*,#10229,.T.);
#15103=ORIENTED_EDGE('',*,*,#10230,.T.);
#15104=ORIENTED_EDGE('',*,*,#10231,.F.);
#15105=ORIENTED_EDGE('',*,*,#10232,.T.);
#15106=ORIENTED_EDGE('',*,*,#10233,.T.);
#15107=ORIENTED_EDGE('',*,*,#10234,.T.);
#15108=ORIENTED_EDGE('',*,*,#10235,.F.);
#15109=ORIENTED_EDGE('',*,*,#10236,.T.);
#15110=ORIENTED_EDGE('',*,*,#10237,.T.);
#15111=ORIENTED_EDGE('',*,*,#10238,.T.);
#15112=ORIENTED_EDGE('',*,*,#10239,.F.);
#15113=ORIENTED_EDGE('',*,*,#10240,.T.);
#15114=ORIENTED_EDGE('',*,*,#10241,.T.);
#15115=ORIENTED_EDGE('',*,*,#10242,.T.);
#15116=ORIENTED_EDGE('',*,*,#10243,.T.);
#15117=ORIENTED_EDGE('',*,*,#10242,.F.);
#15118=ORIENTED_EDGE('',*,*,#10244,.T.);
#15119=ORIENTED_EDGE('',*,*,#10245,.T.);
#15120=ORIENTED_EDGE('',*,*,#10246,.F.);
#15121=ORIENTED_EDGE('',*,*,#10247,.T.);
#15122=ORIENTED_EDGE('',*,*,#10248,.T.);
#15123=ORIENTED_EDGE('',*,*,#10249,.T.);
#15124=ORIENTED_EDGE('',*,*,#10250,.F.);
#15125=ORIENTED_EDGE('',*,*,#10251,.T.);
#15126=ORIENTED_EDGE('',*,*,#10252,.T.);
#15127=ORIENTED_EDGE('',*,*,#10253,.T.);
#15128=ORIENTED_EDGE('',*,*,#10254,.F.);
#15129=ORIENTED_EDGE('',*,*,#10255,.T.);
#15130=ORIENTED_EDGE('',*,*,#10256,.T.);
#15131=ORIENTED_EDGE('',*,*,#10257,.T.);
#15132=ORIENTED_EDGE('',*,*,#10258,.F.);
#15133=ORIENTED_EDGE('',*,*,#10259,.T.);
#15134=ORIENTED_EDGE('',*,*,#10260,.T.);
#15135=ORIENTED_EDGE('',*,*,#10261,.T.);
#15136=ORIENTED_EDGE('',*,*,#10262,.F.);
#15137=ORIENTED_EDGE('',*,*,#10263,.T.);
#15138=ORIENTED_EDGE('',*,*,#10264,.T.);
#15139=ORIENTED_EDGE('',*,*,#10265,.T.);
#15140=ORIENTED_EDGE('',*,*,#10266,.F.);
#15141=ORIENTED_EDGE('',*,*,#10267,.T.);
#15142=ORIENTED_EDGE('',*,*,#10268,.T.);
#15143=ORIENTED_EDGE('',*,*,#10269,.T.);
#15144=ORIENTED_EDGE('',*,*,#10270,.F.);
#15145=ORIENTED_EDGE('',*,*,#10271,.T.);
#15146=ORIENTED_EDGE('',*,*,#10272,.T.);
#15147=ORIENTED_EDGE('',*,*,#10273,.T.);
#15148=ORIENTED_EDGE('',*,*,#10274,.F.);
#15149=ORIENTED_EDGE('',*,*,#10275,.T.);
#15150=ORIENTED_EDGE('',*,*,#10276,.T.);
#15151=ORIENTED_EDGE('',*,*,#10277,.T.);
#15152=ORIENTED_EDGE('',*,*,#10278,.F.);
#15153=ORIENTED_EDGE('',*,*,#10279,.T.);
#15154=ORIENTED_EDGE('',*,*,#10280,.T.);
#15155=ORIENTED_EDGE('',*,*,#10281,.T.);
#15156=ORIENTED_EDGE('',*,*,#10282,.F.);
#15157=ORIENTED_EDGE('',*,*,#10283,.T.);
#15158=ORIENTED_EDGE('',*,*,#10284,.T.);
#15159=ORIENTED_EDGE('',*,*,#10285,.T.);
#15160=ORIENTED_EDGE('',*,*,#10286,.F.);
#15161=ORIENTED_EDGE('',*,*,#10287,.T.);
#15162=ORIENTED_EDGE('',*,*,#10288,.T.);
#15163=ORIENTED_EDGE('',*,*,#10289,.T.);
#15164=ORIENTED_EDGE('',*,*,#10290,.F.);
#15165=ORIENTED_EDGE('',*,*,#10291,.T.);
#15166=ORIENTED_EDGE('',*,*,#10292,.T.);
#15167=ORIENTED_EDGE('',*,*,#10293,.T.);
#15168=ORIENTED_EDGE('',*,*,#10294,.F.);
#15169=ORIENTED_EDGE('',*,*,#10295,.T.);
#15170=ORIENTED_EDGE('',*,*,#10296,.T.);
#15171=ORIENTED_EDGE('',*,*,#10297,.T.);
#15172=ORIENTED_EDGE('',*,*,#10298,.F.);
#15173=ORIENTED_EDGE('',*,*,#10299,.T.);
#15174=ORIENTED_EDGE('',*,*,#10300,.T.);
#15175=ORIENTED_EDGE('',*,*,#10301,.T.);
#15176=ORIENTED_EDGE('',*,*,#10302,.F.);
#15177=ORIENTED_EDGE('',*,*,#10303,.T.);
#15178=ORIENTED_EDGE('',*,*,#10304,.T.);
#15179=ORIENTED_EDGE('',*,*,#10305,.T.);
#15180=ORIENTED_EDGE('',*,*,#10306,.F.);
#15181=ORIENTED_EDGE('',*,*,#10307,.F.);
#15182=ORIENTED_EDGE('',*,*,#10308,.F.);
#15183=ORIENTED_EDGE('',*,*,#10309,.F.);
#15184=ORIENTED_EDGE('',*,*,#10188,.F.);
#15185=ORIENTED_EDGE('',*,*,#10189,.F.);
#15186=ORIENTED_EDGE('',*,*,#10309,.T.);
#15187=ORIENTED_EDGE('',*,*,#10310,.T.);
#15188=ORIENTED_EDGE('',*,*,#10311,.F.);
#15189=ORIENTED_EDGE('',*,*,#10190,.F.);
#15190=ORIENTED_EDGE('',*,*,#10310,.F.);
#15191=ORIENTED_EDGE('',*,*,#10308,.T.);
#15192=ORIENTED_EDGE('',*,*,#10312,.F.);
#15193=ORIENTED_EDGE('',*,*,#10313,.F.);
#15194=ORIENTED_EDGE('',*,*,#10314,.F.);
#15195=ORIENTED_EDGE('',*,*,#10192,.F.);
#15196=ORIENTED_EDGE('',*,*,#10193,.F.);
#15197=ORIENTED_EDGE('',*,*,#10314,.T.);
#15198=ORIENTED_EDGE('',*,*,#10315,.T.);
#15199=ORIENTED_EDGE('',*,*,#10316,.F.);
#15200=ORIENTED_EDGE('',*,*,#10194,.F.);
#15201=ORIENTED_EDGE('',*,*,#10315,.F.);
#15202=ORIENTED_EDGE('',*,*,#10313,.T.);
#15203=ORIENTED_EDGE('',*,*,#10317,.F.);
#15204=ORIENTED_EDGE('',*,*,#10318,.F.);
#15205=ORIENTED_EDGE('',*,*,#10319,.F.);
#15206=ORIENTED_EDGE('',*,*,#10196,.F.);
#15207=ORIENTED_EDGE('',*,*,#10197,.F.);
#15208=ORIENTED_EDGE('',*,*,#10319,.T.);
#15209=ORIENTED_EDGE('',*,*,#10320,.T.);
#15210=ORIENTED_EDGE('',*,*,#10321,.F.);
#15211=ORIENTED_EDGE('',*,*,#10198,.F.);
#15212=ORIENTED_EDGE('',*,*,#10320,.F.);
#15213=ORIENTED_EDGE('',*,*,#10318,.T.);
#15214=ORIENTED_EDGE('',*,*,#10322,.F.);
#15215=ORIENTED_EDGE('',*,*,#10323,.F.);
#15216=ORIENTED_EDGE('',*,*,#10324,.F.);
#15217=ORIENTED_EDGE('',*,*,#10200,.F.);
#15218=ORIENTED_EDGE('',*,*,#10201,.F.);
#15219=ORIENTED_EDGE('',*,*,#10324,.T.);
#15220=ORIENTED_EDGE('',*,*,#10325,.T.);
#15221=ORIENTED_EDGE('',*,*,#10326,.F.);
#15222=ORIENTED_EDGE('',*,*,#10202,.F.);
#15223=ORIENTED_EDGE('',*,*,#10325,.F.);
#15224=ORIENTED_EDGE('',*,*,#10323,.T.);
#15225=ORIENTED_EDGE('',*,*,#10327,.F.);
#15226=ORIENTED_EDGE('',*,*,#10328,.F.);
#15227=ORIENTED_EDGE('',*,*,#10329,.F.);
#15228=ORIENTED_EDGE('',*,*,#10204,.F.);
#15229=ORIENTED_EDGE('',*,*,#10205,.F.);
#15230=ORIENTED_EDGE('',*,*,#10329,.T.);
#15231=ORIENTED_EDGE('',*,*,#10330,.T.);
#15232=ORIENTED_EDGE('',*,*,#10331,.F.);
#15233=ORIENTED_EDGE('',*,*,#10206,.F.);
#15234=ORIENTED_EDGE('',*,*,#10330,.F.);
#15235=ORIENTED_EDGE('',*,*,#10328,.T.);
#15236=ORIENTED_EDGE('',*,*,#10332,.F.);
#15237=ORIENTED_EDGE('',*,*,#10333,.F.);
#15238=ORIENTED_EDGE('',*,*,#10334,.F.);
#15239=ORIENTED_EDGE('',*,*,#10208,.F.);
#15240=ORIENTED_EDGE('',*,*,#10209,.F.);
#15241=ORIENTED_EDGE('',*,*,#10334,.T.);
#15242=ORIENTED_EDGE('',*,*,#10335,.T.);
#15243=ORIENTED_EDGE('',*,*,#10336,.F.);
#15244=ORIENTED_EDGE('',*,*,#10210,.F.);
#15245=ORIENTED_EDGE('',*,*,#10335,.F.);
#15246=ORIENTED_EDGE('',*,*,#10333,.T.);
#15247=ORIENTED_EDGE('',*,*,#10337,.F.);
#15248=ORIENTED_EDGE('',*,*,#10338,.F.);
#15249=ORIENTED_EDGE('',*,*,#10339,.F.);
#15250=ORIENTED_EDGE('',*,*,#10212,.F.);
#15251=ORIENTED_EDGE('',*,*,#10213,.F.);
#15252=ORIENTED_EDGE('',*,*,#10339,.T.);
#15253=ORIENTED_EDGE('',*,*,#10340,.T.);
#15254=ORIENTED_EDGE('',*,*,#10341,.F.);
#15255=ORIENTED_EDGE('',*,*,#10214,.F.);
#15256=ORIENTED_EDGE('',*,*,#10340,.F.);
#15257=ORIENTED_EDGE('',*,*,#10338,.T.);
#15258=ORIENTED_EDGE('',*,*,#10342,.F.);
#15259=ORIENTED_EDGE('',*,*,#10343,.F.);
#15260=ORIENTED_EDGE('',*,*,#10344,.F.);
#15261=ORIENTED_EDGE('',*,*,#10216,.F.);
#15262=ORIENTED_EDGE('',*,*,#10217,.F.);
#15263=ORIENTED_EDGE('',*,*,#10344,.T.);
#15264=ORIENTED_EDGE('',*,*,#10345,.T.);
#15265=ORIENTED_EDGE('',*,*,#10346,.F.);
#15266=ORIENTED_EDGE('',*,*,#10218,.F.);
#15267=ORIENTED_EDGE('',*,*,#10345,.F.);
#15268=ORIENTED_EDGE('',*,*,#10343,.T.);
#15269=ORIENTED_EDGE('',*,*,#10347,.F.);
#15270=ORIENTED_EDGE('',*,*,#10348,.F.);
#15271=ORIENTED_EDGE('',*,*,#10349,.F.);
#15272=ORIENTED_EDGE('',*,*,#10220,.F.);
#15273=ORIENTED_EDGE('',*,*,#10221,.F.);
#15274=ORIENTED_EDGE('',*,*,#10349,.T.);
#15275=ORIENTED_EDGE('',*,*,#10350,.T.);
#15276=ORIENTED_EDGE('',*,*,#10351,.F.);
#15277=ORIENTED_EDGE('',*,*,#10222,.F.);
#15278=ORIENTED_EDGE('',*,*,#10350,.F.);
#15279=ORIENTED_EDGE('',*,*,#10348,.T.);
#15280=ORIENTED_EDGE('',*,*,#10352,.F.);
#15281=ORIENTED_EDGE('',*,*,#10353,.F.);
#15282=ORIENTED_EDGE('',*,*,#10354,.F.);
#15283=ORIENTED_EDGE('',*,*,#10224,.F.);
#15284=ORIENTED_EDGE('',*,*,#10225,.F.);
#15285=ORIENTED_EDGE('',*,*,#10354,.T.);
#15286=ORIENTED_EDGE('',*,*,#10355,.T.);
#15287=ORIENTED_EDGE('',*,*,#10356,.F.);
#15288=ORIENTED_EDGE('',*,*,#10226,.F.);
#15289=ORIENTED_EDGE('',*,*,#10355,.F.);
#15290=ORIENTED_EDGE('',*,*,#10353,.T.);
#15291=ORIENTED_EDGE('',*,*,#10357,.F.);
#15292=ORIENTED_EDGE('',*,*,#10358,.F.);
#15293=ORIENTED_EDGE('',*,*,#10359,.F.);
#15294=ORIENTED_EDGE('',*,*,#10228,.F.);
#15295=ORIENTED_EDGE('',*,*,#10229,.F.);
#15296=ORIENTED_EDGE('',*,*,#10359,.T.);
#15297=ORIENTED_EDGE('',*,*,#10360,.T.);
#15298=ORIENTED_EDGE('',*,*,#10361,.F.);
#15299=ORIENTED_EDGE('',*,*,#10230,.F.);
#15300=ORIENTED_EDGE('',*,*,#10360,.F.);
#15301=ORIENTED_EDGE('',*,*,#10358,.T.);
#15302=ORIENTED_EDGE('',*,*,#10362,.F.);
#15303=ORIENTED_EDGE('',*,*,#10363,.F.);
#15304=ORIENTED_EDGE('',*,*,#10364,.F.);
#15305=ORIENTED_EDGE('',*,*,#10232,.F.);
#15306=ORIENTED_EDGE('',*,*,#10233,.F.);
#15307=ORIENTED_EDGE('',*,*,#10364,.T.);
#15308=ORIENTED_EDGE('',*,*,#10365,.T.);
#15309=ORIENTED_EDGE('',*,*,#10366,.F.);
#15310=ORIENTED_EDGE('',*,*,#10234,.F.);
#15311=ORIENTED_EDGE('',*,*,#10365,.F.);
#15312=ORIENTED_EDGE('',*,*,#10363,.T.);
#15313=ORIENTED_EDGE('',*,*,#10367,.F.);
#15314=ORIENTED_EDGE('',*,*,#10368,.F.);
#15315=ORIENTED_EDGE('',*,*,#10369,.F.);
#15316=ORIENTED_EDGE('',*,*,#10236,.F.);
#15317=ORIENTED_EDGE('',*,*,#10237,.F.);
#15318=ORIENTED_EDGE('',*,*,#10369,.T.);
#15319=ORIENTED_EDGE('',*,*,#10370,.T.);
#15320=ORIENTED_EDGE('',*,*,#10371,.F.);
#15321=ORIENTED_EDGE('',*,*,#10238,.F.);
#15322=ORIENTED_EDGE('',*,*,#10370,.F.);
#15323=ORIENTED_EDGE('',*,*,#10368,.T.);
#15324=ORIENTED_EDGE('',*,*,#10372,.F.);
#15325=ORIENTED_EDGE('',*,*,#10373,.F.);
#15326=ORIENTED_EDGE('',*,*,#10374,.F.);
#15327=ORIENTED_EDGE('',*,*,#10240,.F.);
#15328=ORIENTED_EDGE('',*,*,#10241,.F.);
#15329=ORIENTED_EDGE('',*,*,#10374,.T.);
#15330=ORIENTED_EDGE('',*,*,#10375,.T.);
#15331=ORIENTED_EDGE('',*,*,#10244,.F.);
#15332=ORIENTED_EDGE('',*,*,#10376,.F.);
#15333=ORIENTED_EDGE('',*,*,#10245,.F.);
#15334=ORIENTED_EDGE('',*,*,#10375,.F.);
#15335=ORIENTED_EDGE('',*,*,#10373,.T.);
#15336=ORIENTED_EDGE('',*,*,#10377,.F.);
#15337=ORIENTED_EDGE('',*,*,#10378,.F.);
#15338=ORIENTED_EDGE('',*,*,#10379,.F.);
#15339=ORIENTED_EDGE('',*,*,#10247,.F.);
#15340=ORIENTED_EDGE('',*,*,#10248,.F.);
#15341=ORIENTED_EDGE('',*,*,#10379,.T.);
#15342=ORIENTED_EDGE('',*,*,#10380,.T.);
#15343=ORIENTED_EDGE('',*,*,#10381,.F.);
#15344=ORIENTED_EDGE('',*,*,#10249,.F.);
#15345=ORIENTED_EDGE('',*,*,#10380,.F.);
#15346=ORIENTED_EDGE('',*,*,#10378,.T.);
#15347=ORIENTED_EDGE('',*,*,#10382,.F.);
#15348=ORIENTED_EDGE('',*,*,#10383,.F.);
#15349=ORIENTED_EDGE('',*,*,#10384,.F.);
#15350=ORIENTED_EDGE('',*,*,#10251,.F.);
#15351=ORIENTED_EDGE('',*,*,#10252,.F.);
#15352=ORIENTED_EDGE('',*,*,#10384,.T.);
#15353=ORIENTED_EDGE('',*,*,#10385,.T.);
#15354=ORIENTED_EDGE('',*,*,#10386,.F.);
#15355=ORIENTED_EDGE('',*,*,#10253,.F.);
#15356=ORIENTED_EDGE('',*,*,#10385,.F.);
#15357=ORIENTED_EDGE('',*,*,#10383,.T.);
#15358=ORIENTED_EDGE('',*,*,#10387,.F.);
#15359=ORIENTED_EDGE('',*,*,#10388,.F.);
#15360=ORIENTED_EDGE('',*,*,#10389,.F.);
#15361=ORIENTED_EDGE('',*,*,#10255,.F.);
#15362=ORIENTED_EDGE('',*,*,#10256,.F.);
#15363=ORIENTED_EDGE('',*,*,#10389,.T.);
#15364=ORIENTED_EDGE('',*,*,#10390,.T.);
#15365=ORIENTED_EDGE('',*,*,#10391,.F.);
#15366=ORIENTED_EDGE('',*,*,#10257,.F.);
#15367=ORIENTED_EDGE('',*,*,#10390,.F.);
#15368=ORIENTED_EDGE('',*,*,#10388,.T.);
#15369=ORIENTED_EDGE('',*,*,#10392,.F.);
#15370=ORIENTED_EDGE('',*,*,#10393,.F.);
#15371=ORIENTED_EDGE('',*,*,#10394,.F.);
#15372=ORIENTED_EDGE('',*,*,#10259,.F.);
#15373=ORIENTED_EDGE('',*,*,#10260,.F.);
#15374=ORIENTED_EDGE('',*,*,#10394,.T.);
#15375=ORIENTED_EDGE('',*,*,#10395,.T.);
#15376=ORIENTED_EDGE('',*,*,#10396,.F.);
#15377=ORIENTED_EDGE('',*,*,#10261,.F.);
#15378=ORIENTED_EDGE('',*,*,#10395,.F.);
#15379=ORIENTED_EDGE('',*,*,#10393,.T.);
#15380=ORIENTED_EDGE('',*,*,#10397,.F.);
#15381=ORIENTED_EDGE('',*,*,#10398,.F.);
#15382=ORIENTED_EDGE('',*,*,#10399,.F.);
#15383=ORIENTED_EDGE('',*,*,#10263,.F.);
#15384=ORIENTED_EDGE('',*,*,#10264,.F.);
#15385=ORIENTED_EDGE('',*,*,#10399,.T.);
#15386=ORIENTED_EDGE('',*,*,#10400,.T.);
#15387=ORIENTED_EDGE('',*,*,#10401,.F.);
#15388=ORIENTED_EDGE('',*,*,#10265,.F.);
#15389=ORIENTED_EDGE('',*,*,#10400,.F.);
#15390=ORIENTED_EDGE('',*,*,#10398,.T.);
#15391=ORIENTED_EDGE('',*,*,#10402,.F.);
#15392=ORIENTED_EDGE('',*,*,#10403,.F.);
#15393=ORIENTED_EDGE('',*,*,#10404,.F.);
#15394=ORIENTED_EDGE('',*,*,#10267,.F.);
#15395=ORIENTED_EDGE('',*,*,#10268,.F.);
#15396=ORIENTED_EDGE('',*,*,#10404,.T.);
#15397=ORIENTED_EDGE('',*,*,#10405,.T.);
#15398=ORIENTED_EDGE('',*,*,#10406,.F.);
#15399=ORIENTED_EDGE('',*,*,#10269,.F.);
#15400=ORIENTED_EDGE('',*,*,#10405,.F.);
#15401=ORIENTED_EDGE('',*,*,#10403,.T.);
#15402=ORIENTED_EDGE('',*,*,#10407,.F.);
#15403=ORIENTED_EDGE('',*,*,#10408,.F.);
#15404=ORIENTED_EDGE('',*,*,#10409,.F.);
#15405=ORIENTED_EDGE('',*,*,#10271,.F.);
#15406=ORIENTED_EDGE('',*,*,#10272,.F.);
#15407=ORIENTED_EDGE('',*,*,#10409,.T.);
#15408=ORIENTED_EDGE('',*,*,#10410,.T.);
#15409=ORIENTED_EDGE('',*,*,#10411,.F.);
#15410=ORIENTED_EDGE('',*,*,#10273,.F.);
#15411=ORIENTED_EDGE('',*,*,#10410,.F.);
#15412=ORIENTED_EDGE('',*,*,#10408,.T.);
#15413=ORIENTED_EDGE('',*,*,#10412,.F.);
#15414=ORIENTED_EDGE('',*,*,#10413,.F.);
#15415=ORIENTED_EDGE('',*,*,#10414,.F.);
#15416=ORIENTED_EDGE('',*,*,#10275,.F.);
#15417=ORIENTED_EDGE('',*,*,#10276,.F.);
#15418=ORIENTED_EDGE('',*,*,#10414,.T.);
#15419=ORIENTED_EDGE('',*,*,#10415,.T.);
#15420=ORIENTED_EDGE('',*,*,#10416,.F.);
#15421=ORIENTED_EDGE('',*,*,#10277,.F.);
#15422=ORIENTED_EDGE('',*,*,#10415,.F.);
#15423=ORIENTED_EDGE('',*,*,#10413,.T.);
#15424=ORIENTED_EDGE('',*,*,#10417,.F.);
#15425=ORIENTED_EDGE('',*,*,#10418,.F.);
#15426=ORIENTED_EDGE('',*,*,#10419,.F.);
#15427=ORIENTED_EDGE('',*,*,#10279,.F.);
#15428=ORIENTED_EDGE('',*,*,#10280,.F.);
#15429=ORIENTED_EDGE('',*,*,#10419,.T.);
#15430=ORIENTED_EDGE('',*,*,#10420,.T.);
#15431=ORIENTED_EDGE('',*,*,#10421,.F.);
#15432=ORIENTED_EDGE('',*,*,#10281,.F.);
#15433=ORIENTED_EDGE('',*,*,#10420,.F.);
#15434=ORIENTED_EDGE('',*,*,#10418,.T.);
#15435=ORIENTED_EDGE('',*,*,#10422,.F.);
#15436=ORIENTED_EDGE('',*,*,#10423,.F.);
#15437=ORIENTED_EDGE('',*,*,#10424,.F.);
#15438=ORIENTED_EDGE('',*,*,#10283,.F.);
#15439=ORIENTED_EDGE('',*,*,#10284,.F.);
#15440=ORIENTED_EDGE('',*,*,#10424,.T.);
#15441=ORIENTED_EDGE('',*,*,#10425,.T.);
#15442=ORIENTED_EDGE('',*,*,#10426,.F.);
#15443=ORIENTED_EDGE('',*,*,#10285,.F.);
#15444=ORIENTED_EDGE('',*,*,#10425,.F.);
#15445=ORIENTED_EDGE('',*,*,#10423,.T.);
#15446=ORIENTED_EDGE('',*,*,#10427,.F.);
#15447=ORIENTED_EDGE('',*,*,#10428,.F.);
#15448=ORIENTED_EDGE('',*,*,#10429,.F.);
#15449=ORIENTED_EDGE('',*,*,#10287,.F.);
#15450=ORIENTED_EDGE('',*,*,#10288,.F.);
#15451=ORIENTED_EDGE('',*,*,#10429,.T.);
#15452=ORIENTED_EDGE('',*,*,#10430,.T.);
#15453=ORIENTED_EDGE('',*,*,#10431,.F.);
#15454=ORIENTED_EDGE('',*,*,#10289,.F.);
#15455=ORIENTED_EDGE('',*,*,#10430,.F.);
#15456=ORIENTED_EDGE('',*,*,#10428,.T.);
#15457=ORIENTED_EDGE('',*,*,#10432,.F.);
#15458=ORIENTED_EDGE('',*,*,#10433,.F.);
#15459=ORIENTED_EDGE('',*,*,#10434,.F.);
#15460=ORIENTED_EDGE('',*,*,#10291,.F.);
#15461=ORIENTED_EDGE('',*,*,#10292,.F.);
#15462=ORIENTED_EDGE('',*,*,#10434,.T.);
#15463=ORIENTED_EDGE('',*,*,#10435,.T.);
#15464=ORIENTED_EDGE('',*,*,#10436,.F.);
#15465=ORIENTED_EDGE('',*,*,#10293,.F.);
#15466=ORIENTED_EDGE('',*,*,#10435,.F.);
#15467=ORIENTED_EDGE('',*,*,#10433,.T.);
#15468=ORIENTED_EDGE('',*,*,#10437,.F.);
#15469=ORIENTED_EDGE('',*,*,#10438,.F.);
#15470=ORIENTED_EDGE('',*,*,#10439,.F.);
#15471=ORIENTED_EDGE('',*,*,#10295,.F.);
#15472=ORIENTED_EDGE('',*,*,#10296,.F.);
#15473=ORIENTED_EDGE('',*,*,#10439,.T.);
#15474=ORIENTED_EDGE('',*,*,#10440,.T.);
#15475=ORIENTED_EDGE('',*,*,#10441,.F.);
#15476=ORIENTED_EDGE('',*,*,#10297,.F.);
#15477=ORIENTED_EDGE('',*,*,#10440,.F.);
#15478=ORIENTED_EDGE('',*,*,#10438,.T.);
#15479=ORIENTED_EDGE('',*,*,#10442,.F.);
#15480=ORIENTED_EDGE('',*,*,#10443,.F.);
#15481=ORIENTED_EDGE('',*,*,#10444,.F.);
#15482=ORIENTED_EDGE('',*,*,#10299,.F.);
#15483=ORIENTED_EDGE('',*,*,#10300,.F.);
#15484=ORIENTED_EDGE('',*,*,#10444,.T.);
#15485=ORIENTED_EDGE('',*,*,#10445,.T.);
#15486=ORIENTED_EDGE('',*,*,#10446,.F.);
#15487=ORIENTED_EDGE('',*,*,#10301,.F.);
#15488=ORIENTED_EDGE('',*,*,#10445,.F.);
#15489=ORIENTED_EDGE('',*,*,#10443,.T.);
#15490=ORIENTED_EDGE('',*,*,#10447,.F.);
#15491=ORIENTED_EDGE('',*,*,#10448,.F.);
#15492=ORIENTED_EDGE('',*,*,#10449,.F.);
#15493=ORIENTED_EDGE('',*,*,#10303,.F.);
#15494=ORIENTED_EDGE('',*,*,#10304,.F.);
#15495=ORIENTED_EDGE('',*,*,#10449,.T.);
#15496=ORIENTED_EDGE('',*,*,#10450,.T.);
#15497=ORIENTED_EDGE('',*,*,#10451,.F.);
#15498=ORIENTED_EDGE('',*,*,#10305,.F.);
#15499=ORIENTED_EDGE('',*,*,#10450,.F.);
#15500=ORIENTED_EDGE('',*,*,#10448,.T.);
#15501=ORIENTED_EDGE('',*,*,#10452,.F.);
#15502=ORIENTED_EDGE('',*,*,#10172,.F.);
#15503=ORIENTED_EDGE('',*,*,#10081,.F.);
#15504=ORIENTED_EDGE('',*,*,#10173,.F.);
#15505=ORIENTED_EDGE('',*,*,#10453,.T.);
#15506=ORIENTED_EDGE('',*,*,#10452,.T.);
#15507=ORIENTED_EDGE('',*,*,#10453,.F.);
#15508=ORIENTED_EDGE('',*,*,#10122,.T.);
#15509=ORIENTED_EDGE('',*,*,#10169,.T.);
#15510=ORIENTED_EDGE('',*,*,#10454,.F.);
#15511=ORIENTED_EDGE('',*,*,#10178,.T.);
#15512=ORIENTED_EDGE('',*,*,#10455,.F.);
#15513=ORIENTED_EDGE('',*,*,#10454,.T.);
#15514=ORIENTED_EDGE('',*,*,#10168,.T.);
#15515=ORIENTED_EDGE('',*,*,#10127,.T.);
#15516=ORIENTED_EDGE('',*,*,#10177,.T.);
#15517=ORIENTED_EDGE('',*,*,#10243,.F.);
#15518=ORIENTED_EDGE('',*,*,#10456,.T.);
#15519=ORIENTED_EDGE('',*,*,#10455,.T.);
#15520=ORIENTED_EDGE('',*,*,#10456,.F.);
#15521=ORIENTED_EDGE('',*,*,#10457,.F.);
#15522=ORIENTED_EDGE('',*,*,#10458,.T.);
#15523=ORIENTED_EDGE('',*,*,#10372,.T.);
#15524=ORIENTED_EDGE('',*,*,#10239,.T.);
#15525=ORIENTED_EDGE('',*,*,#10371,.T.);
#15526=ORIENTED_EDGE('',*,*,#10367,.T.);
#15527=ORIENTED_EDGE('',*,*,#10235,.T.);
#15528=ORIENTED_EDGE('',*,*,#10366,.T.);
#15529=ORIENTED_EDGE('',*,*,#10362,.T.);
#15530=ORIENTED_EDGE('',*,*,#10231,.T.);
#15531=ORIENTED_EDGE('',*,*,#10361,.T.);
#15532=ORIENTED_EDGE('',*,*,#10357,.T.);
#15533=ORIENTED_EDGE('',*,*,#10227,.T.);
#15534=ORIENTED_EDGE('',*,*,#10356,.T.);
#15535=ORIENTED_EDGE('',*,*,#10352,.T.);
#15536=ORIENTED_EDGE('',*,*,#10223,.T.);
#15537=ORIENTED_EDGE('',*,*,#10351,.T.);
#15538=ORIENTED_EDGE('',*,*,#10347,.T.);
#15539=ORIENTED_EDGE('',*,*,#10219,.T.);
#15540=ORIENTED_EDGE('',*,*,#10346,.T.);
#15541=ORIENTED_EDGE('',*,*,#10342,.T.);
#15542=ORIENTED_EDGE('',*,*,#10215,.T.);
#15543=ORIENTED_EDGE('',*,*,#10341,.T.);
#15544=ORIENTED_EDGE('',*,*,#10337,.T.);
#15545=ORIENTED_EDGE('',*,*,#10211,.T.);
#15546=ORIENTED_EDGE('',*,*,#10336,.T.);
#15547=ORIENTED_EDGE('',*,*,#10332,.T.);
#15548=ORIENTED_EDGE('',*,*,#10207,.T.);
#15549=ORIENTED_EDGE('',*,*,#10331,.T.);
#15550=ORIENTED_EDGE('',*,*,#10327,.T.);
#15551=ORIENTED_EDGE('',*,*,#10203,.T.);
#15552=ORIENTED_EDGE('',*,*,#10326,.T.);
#15553=ORIENTED_EDGE('',*,*,#10322,.T.);
#15554=ORIENTED_EDGE('',*,*,#10199,.T.);
#15555=ORIENTED_EDGE('',*,*,#10321,.T.);
#15556=ORIENTED_EDGE('',*,*,#10317,.T.);
#15557=ORIENTED_EDGE('',*,*,#10195,.T.);
#15558=ORIENTED_EDGE('',*,*,#10316,.T.);
#15559=ORIENTED_EDGE('',*,*,#10312,.T.);
#15560=ORIENTED_EDGE('',*,*,#10191,.T.);
#15561=ORIENTED_EDGE('',*,*,#10311,.T.);
#15562=ORIENTED_EDGE('',*,*,#10307,.T.);
#15563=ORIENTED_EDGE('',*,*,#10187,.T.);
#15564=ORIENTED_EDGE('',*,*,#10185,.T.);
#15565=ORIENTED_EDGE('',*,*,#10179,.T.);
#15566=ORIENTED_EDGE('',*,*,#10306,.T.);
#15567=ORIENTED_EDGE('',*,*,#10451,.T.);
#15568=ORIENTED_EDGE('',*,*,#10447,.T.);
#15569=ORIENTED_EDGE('',*,*,#10302,.T.);
#15570=ORIENTED_EDGE('',*,*,#10446,.T.);
#15571=ORIENTED_EDGE('',*,*,#10442,.T.);
#15572=ORIENTED_EDGE('',*,*,#10298,.T.);
#15573=ORIENTED_EDGE('',*,*,#10441,.T.);
#15574=ORIENTED_EDGE('',*,*,#10437,.T.);
#15575=ORIENTED_EDGE('',*,*,#10294,.T.);
#15576=ORIENTED_EDGE('',*,*,#10436,.T.);
#15577=ORIENTED_EDGE('',*,*,#10432,.T.);
#15578=ORIENTED_EDGE('',*,*,#10290,.T.);
#15579=ORIENTED_EDGE('',*,*,#10431,.T.);
#15580=ORIENTED_EDGE('',*,*,#10427,.T.);
#15581=ORIENTED_EDGE('',*,*,#10286,.T.);
#15582=ORIENTED_EDGE('',*,*,#10426,.T.);
#15583=ORIENTED_EDGE('',*,*,#10422,.T.);
#15584=ORIENTED_EDGE('',*,*,#10282,.T.);
#15585=ORIENTED_EDGE('',*,*,#10421,.T.);
#15586=ORIENTED_EDGE('',*,*,#10417,.T.);
#15587=ORIENTED_EDGE('',*,*,#10278,.T.);
#15588=ORIENTED_EDGE('',*,*,#10416,.T.);
#15589=ORIENTED_EDGE('',*,*,#10412,.T.);
#15590=ORIENTED_EDGE('',*,*,#10274,.T.);
#15591=ORIENTED_EDGE('',*,*,#10411,.T.);
#15592=ORIENTED_EDGE('',*,*,#10407,.T.);
#15593=ORIENTED_EDGE('',*,*,#10270,.T.);
#15594=ORIENTED_EDGE('',*,*,#10406,.T.);
#15595=ORIENTED_EDGE('',*,*,#10402,.T.);
#15596=ORIENTED_EDGE('',*,*,#10266,.T.);
#15597=ORIENTED_EDGE('',*,*,#10401,.T.);
#15598=ORIENTED_EDGE('',*,*,#10397,.T.);
#15599=ORIENTED_EDGE('',*,*,#10262,.T.);
#15600=ORIENTED_EDGE('',*,*,#10396,.T.);
#15601=ORIENTED_EDGE('',*,*,#10392,.T.);
#15602=ORIENTED_EDGE('',*,*,#10258,.T.);
#15603=ORIENTED_EDGE('',*,*,#10391,.T.);
#15604=ORIENTED_EDGE('',*,*,#10387,.T.);
#15605=ORIENTED_EDGE('',*,*,#10254,.T.);
#15606=ORIENTED_EDGE('',*,*,#10386,.T.);
#15607=ORIENTED_EDGE('',*,*,#10382,.T.);
#15608=ORIENTED_EDGE('',*,*,#10250,.T.);
#15609=ORIENTED_EDGE('',*,*,#10381,.T.);
#15610=ORIENTED_EDGE('',*,*,#10377,.T.);
#15611=ORIENTED_EDGE('',*,*,#10246,.T.);
#15612=ORIENTED_EDGE('',*,*,#10376,.T.);
#15613=ORIENTED_EDGE('',*,*,#10458,.F.);
#15614=ORIENTED_EDGE('',*,*,#10457,.T.);
#15615=PLANE('',#17219);
#15616=PLANE('',#17220);
#15617=PLANE('',#17221);
#15618=PLANE('',#17222);
#15619=PLANE('',#17223);
#15620=PLANE('',#17224);
#15621=PLANE('',#17225);
#15622=PLANE('',#17228);
#15623=PLANE('',#17229);
#15624=PLANE('',#17230);
#15625=PLANE('',#17231);
#15626=PLANE('',#17232);
#15627=PLANE('',#17233);
#15628=PLANE('',#17234);
#15629=PLANE('',#17235);
#15630=PLANE('',#17236);
#15631=PLANE('',#17237);
#15632=PLANE('',#17238);
#15633=PLANE('',#17239);
#15634=PLANE('',#17240);
#15635=PLANE('',#17241);
#15636=PLANE('',#17242);
#15637=PLANE('',#17243);
#15638=PLANE('',#17245);
#15639=PLANE('',#17246);
#15640=PLANE('',#17248);
#15641=PLANE('',#17249);
#15642=PLANE('',#17250);
#15643=PLANE('',#17251);
#15644=PLANE('',#17253);
#15645=PLANE('',#17262);
#15646=PLANE('',#17269);
#15647=PLANE('',#17270);
#15648=PLANE('',#17271);
#15649=PLANE('',#17272);
#15650=PLANE('',#17273);
#15651=PLANE('',#17274);
#15652=PLANE('',#17275);
#15653=PLANE('',#17276);
#15654=PLANE('',#17277);
#15655=PLANE('',#17278);
#15656=PLANE('',#17283);
#15657=PLANE('',#17284);
#15658=PLANE('',#17286);
#15659=PLANE('',#17287);
#15660=PLANE('',#17288);
#15661=PLANE('',#17289);
#15662=PLANE('',#17303);
#15663=PLANE('',#17310);
#15664=PLANE('',#17311);
#15665=PLANE('',#17316);
#15666=PLANE('',#17317);
#15667=PLANE('',#17318);
#15668=PLANE('',#17319);
#15669=PLANE('',#17320);
#15670=PLANE('',#17321);
#15671=PLANE('',#17322);
#15672=PLANE('',#17324);
#15673=PLANE('',#17330);
#15674=PLANE('',#17336);
#15675=PLANE('',#17340);
#15676=PLANE('',#17346);
#15677=PLANE('',#17352);
#15678=PLANE('',#17358);
#15679=PLANE('',#17359);
#15680=PLANE('',#17360);
#15681=PLANE('',#17367);
#15682=PLANE('',#17373);
#15683=PLANE('',#17379);
#15684=PLANE('',#17380);
#15685=PLANE('',#17386);
#15686=PLANE('',#17387);
#15687=PLANE('',#17393);
#15688=PLANE('',#17394);
#15689=PLANE('',#17400);
#15690=PLANE('',#17401);
#15691=PLANE('',#17407);
#15692=PLANE('',#17408);
#15693=PLANE('',#17414);
#15694=PLANE('',#17415);
#15695=PLANE('',#17421);
#15696=PLANE('',#17422);
#15697=PLANE('',#17428);
#15698=PLANE('',#17441);
#15699=PLANE('',#17604);
#15700=PLANE('',#17605);
#15701=PLANE('',#17610);
#15702=PLANE('',#17611);
#15703=PLANE('',#17616);
#15704=PLANE('',#17617);
#15705=PLANE('',#17622);
#15706=PLANE('',#17627);
#15707=PLANE('',#17628);
#15708=PLANE('',#17633);
#15709=PLANE('',#17634);
#15710=PLANE('',#17639);
#15711=PLANE('',#17640);
#15712=PLANE('',#17645);
#15713=PLANE('',#17646);
#15714=PLANE('',#17651);
#15715=PLANE('',#17652);
#15716=PLANE('',#17657);
#15717=PLANE('',#17658);
#15718=PLANE('',#17663);
#15719=PLANE('',#17676);
#15720=PLANE('',#17699);
#15721=PLANE('',#17704);
#15722=PLANE('',#17707);
#15723=PLANE('',#17712);
#15724=PLANE('',#17713);
#15725=PLANE('',#17718);
#15726=PLANE('',#17719);
#15727=PLANE('',#17724);
#15728=PLANE('',#17729);
#15729=PLANE('',#17730);
#15730=PLANE('',#17735);
#15731=PLANE('',#17736);
#15732=PLANE('',#17741);
#15733=PLANE('',#17742);
#15734=PLANE('',#17747);
#15735=PLANE('',#17748);
#15736=PLANE('',#17753);
#15737=PLANE('',#17754);
#15738=PLANE('',#17759);
#15739=PLANE('',#17774);
#15740=PLANE('',#17793);
#15741=PLANE('',#17798);
#15742=PLANE('',#17799);
#15743=PLANE('',#17804);
#15744=PLANE('',#17805);
#15745=PLANE('',#17810);
#15746=PLANE('',#17811);
#15747=PLANE('',#17816);
#15748=PLANE('',#17817);
#15749=PLANE('',#17822);
#15750=PLANE('',#17827);
#15751=PLANE('',#17828);
#15752=PLANE('',#17833);
#15753=PLANE('',#17834);
#15754=PLANE('',#17839);
#15755=PLANE('',#17840);
#15756=PLANE('',#17845);
#15757=PLANE('',#17846);
#15758=PLANE('',#17851);
#15759=PLANE('',#17872);
#15760=PLANE('',#17887);
#15761=PLANE('',#17892);
#15762=PLANE('',#17895);
#15763=PLANE('',#17900);
#15764=PLANE('',#17901);
#15765=PLANE('',#17906);
#15766=PLANE('',#17907);
#15767=PLANE('',#17912);
#15768=PLANE('',#17913);
#15769=PLANE('',#17918);
#15770=PLANE('',#17919);
#15771=PLANE('',#17924);
#15772=PLANE('',#17929);
#15773=PLANE('',#17930);
#15774=PLANE('',#17935);
#15775=PLANE('',#17936);
#15776=PLANE('',#17941);
#15777=PLANE('',#17942);
#15778=PLANE('',#17947);
#15779=PLANE('',#17970);
#15780=PLANE('',#17981);
#15781=PLANE('',#17986);
#15782=PLANE('',#17987);
#15783=PLANE('',#17992);
#15784=PLANE('',#17993);
#15785=PLANE('',#17998);
#15786=PLANE('',#17999);
#15787=PLANE('',#18004);
#15788=PLANE('',#18005);
#15789=PLANE('',#18010);
#15790=PLANE('',#18011);
#15791=PLANE('',#18016);
#15792=PLANE('',#18017);
#15793=PLANE('',#18022);
#15794=PLANE('',#18027);
#15795=PLANE('',#18028);
#15796=PLANE('',#18033);
#15797=PLANE('',#18034);
#15798=PLANE('',#18039);
#15799=PLANE('',#18068);
#15800=PLANE('',#18075);
#15801=PLANE('',#18080);
#15802=PLANE('',#18081);
#15803=PLANE('',#18086);
#15804=PLANE('',#18087);
#15805=PLANE('',#18092);
#15806=PLANE('',#18093);
#15807=PLANE('',#18098);
#15808=PLANE('',#18099);
#15809=PLANE('',#18104);
#15810=PLANE('',#18105);
#15811=PLANE('',#18110);
#15812=PLANE('',#18111);
#15813=PLANE('',#18116);
#15814=PLANE('',#18117);
#15815=PLANE('',#18122);
#15816=PLANE('',#18127);
#15817=PLANE('',#18128);
#15818=PLANE('',#18133);
#15819=PLANE('',#18166);
#15820=PLANE('',#18169);
#15821=PLANE('',#18174);
#15822=PLANE('',#18175);
#15823=PLANE('',#18180);
#15824=PLANE('',#18181);
#15825=PLANE('',#18186);
#15826=PLANE('',#18187);
#15827=PLANE('',#18192);
#15828=PLANE('',#18193);
#15829=PLANE('',#18198);
#15830=PLANE('',#18199);
#15831=PLANE('',#18204);
#15832=PLANE('',#18205);
#15833=PLANE('',#18210);
#15834=PLANE('',#18211);
#15835=PLANE('',#18216);
#15836=PLANE('',#18217);
#15837=PLANE('',#18222);
#15838=PLANE('',#18227);
#15839=PLANE('',#18264);
#15840=PLANE('',#18299);
#15841=PLANE('',#18302);
#15842=PLANE('',#18305);
#15843=PLANE('',#18308);
#15844=PLANE('',#18311);
#15845=PLANE('',#18314);
#15846=PLANE('',#18317);
#15847=PLANE('',#18320);
#15848=PLANE('',#18323);
#15849=PLANE('',#18326);
#15850=PLANE('',#18329);
#15851=PLANE('',#18332);
#15852=PLANE('',#18335);
#15853=PLANE('',#18339);
#15854=PLANE('',#18446);
#15855=PLANE('',#18484);
#15856=PLANE('',#18485);
#15857=PLANE('',#18486);
#15858=PLANE('',#18487);
#15859=PLANE('',#18488);
#15860=PLANE('',#18489);
#15861=PLANE('',#18492);
#15862=PLANE('',#18493);
#15863=PLANE('',#18494);
#15864=PLANE('',#18495);
#15865=PLANE('',#18496);
#15866=PLANE('',#18497);
#15867=PLANE('',#18498);
#15868=PLANE('',#18499);
#15869=PLANE('',#18500);
#15870=PLANE('',#18501);
#15871=PLANE('',#18504);
#15872=PLANE('',#18505);
#15873=PLANE('',#18506);
#15874=PLANE('',#18507);
#15875=PLANE('',#18508);
#15876=PLANE('',#18509);
#15877=PLANE('',#18510);
#15878=PLANE('',#18511);
#15879=PLANE('',#18512);
#15880=PLANE('',#18513);
#15881=PLANE('',#18516);
#15882=PLANE('',#18517);
#15883=PLANE('',#18518);
#15884=PLANE('',#18519);
#15885=PLANE('',#18520);
#15886=PLANE('',#18521);
#15887=PLANE('',#18522);
#15888=PLANE('',#18523);
#15889=PLANE('',#18524);
#15890=PLANE('',#18525);
#15891=PLANE('',#18526);
#15892=PLANE('',#18527);
#15893=PLANE('',#18528);
#15894=PLANE('',#18529);
#15895=PLANE('',#18530);
#15896=PLANE('',#18531);
#15897=PLANE('',#18532);
#15898=PLANE('',#18533);
#15899=PLANE('',#18534);
#15900=PLANE('',#18535);
#15901=PLANE('',#18536);
#15902=PLANE('',#18537);
#15903=PLANE('',#18538);
#15904=PLANE('',#18539);
#15905=PLANE('',#18540);
#15906=PLANE('',#18541);
#15907=PLANE('',#18542);
#15908=PLANE('',#18543);
#15909=PLANE('',#18544);
#15910=PLANE('',#18545);
#15911=PLANE('',#18546);
#15912=PLANE('',#18547);
#15913=PLANE('',#18548);
#15914=PLANE('',#18549);
#15915=PLANE('',#18550);
#15916=PLANE('',#18551);
#15917=PLANE('',#18552);
#15918=PLANE('',#18553);
#15919=PLANE('',#18554);
#15920=PLANE('',#18555);
#15921=PLANE('',#18556);
#15922=PLANE('',#18559);
#15923=PLANE('',#18560);
#15924=PLANE('',#18561);
#15925=PLANE('',#18562);
#15926=PLANE('',#18563);
#15927=PLANE('',#18564);
#15928=PLANE('',#18565);
#15929=PLANE('',#18566);
#15930=PLANE('',#18567);
#15931=PLANE('',#18570);
#15932=PLANE('',#18571);
#15933=PLANE('',#18572);
#15934=PLANE('',#18573);
#15935=PLANE('',#18574);
#15936=PLANE('',#18575);
#15937=PLANE('',#18576);
#15938=PLANE('',#18577);
#15939=PLANE('',#18578);
#15940=PLANE('',#18579);
#15941=PLANE('',#18582);
#15942=PLANE('',#18583);
#15943=PLANE('',#18584);
#15944=PLANE('',#18585);
#15945=PLANE('',#18598);
#15946=PLANE('',#18629);
#15947=PLANE('',#18634);
#15948=PLANE('',#18640);
#15949=PLANE('',#18656);
#15950=PLANE('',#18663);
#15951=PLANE('',#18669);
#15952=PLANE('',#18672);
#15953=PLANE('',#18683);
#15954=PLANE('',#18690);
#15955=PLANE('',#18694);
#15956=PLANE('',#18697);
#15957=PLANE('',#18698);
#15958=PLANE('',#18703);
#15959=PLANE('',#18707);
#15960=PLANE('',#18715);
#15961=PLANE('',#18719);
#15962=PLANE('',#18728);
#15963=PLANE('',#18732);
#15964=PLANE('',#18747);
#15965=PLANE('',#18748);
#15966=PLANE('',#18749);
#15967=PLANE('',#18750);
#15968=PLANE('',#18751);
#15969=PLANE('',#18752);
#15970=PLANE('',#18753);
#15971=PLANE('',#18754);
#15972=PLANE('',#18755);
#15973=PLANE('',#18756);
#15974=PLANE('',#18757);
#15975=PLANE('',#18758);
#15976=PLANE('',#18759);
#15977=PLANE('',#18760);
#15978=PLANE('',#18761);
#15979=PLANE('',#18763);
#15980=PLANE('',#18764);
#15981=PLANE('',#18765);
#15982=PLANE('',#18772);
#15983=PLANE('',#18773);
#15984=PLANE('',#18785);
#15985=PLANE('',#18788);
#15986=PLANE('',#18793);
#15987=PLANE('',#18794);
#15988=PLANE('',#18795);
#15989=PLANE('',#18796);
#15990=PLANE('',#18797);
#15991=PLANE('',#18798);
#15992=PLANE('',#18799);
#15993=PLANE('',#18800);
#15994=PLANE('',#18807);
#15995=PLANE('',#18840);
#15996=PLANE('',#18845);
#15997=PLANE('',#18846);
#15998=PLANE('',#18848);
#15999=PLANE('',#18911);
#16000=PLANE('',#18912);
#16001=PLANE('',#18913);
#16002=PLANE('',#18914);
#16003=PLANE('',#18915);
#16004=PLANE('',#18916);
#16005=PLANE('',#18917);
#16006=PLANE('',#18918);
#16007=PLANE('',#18919);
#16008=PLANE('',#18920);
#16009=PLANE('',#18921);
#16010=PLANE('',#18922);
#16011=PLANE('',#18923);
#16012=PLANE('',#18924);
#16013=PLANE('',#18925);
#16014=PLANE('',#18926);
#16015=PLANE('',#18927);
#16016=PLANE('',#18928);
#16017=PLANE('',#18929);
#16018=PLANE('',#18930);
#16019=PLANE('',#18931);
#16020=PLANE('',#18932);
#16021=PLANE('',#18933);
#16022=PLANE('',#18934);
#16023=PLANE('',#18935);
#16024=PLANE('',#18936);
#16025=PLANE('',#18937);
#16026=PLANE('',#18938);
#16027=PLANE('',#18939);
#16028=PLANE('',#18940);
#16029=PLANE('',#18941);
#16030=PLANE('',#18942);
#16031=PLANE('',#18943);
#16032=PLANE('',#18944);
#16033=PLANE('',#18945);
#16034=PLANE('',#18946);
#16035=PLANE('',#18947);
#16036=PLANE('',#18948);
#16037=PLANE('',#18949);
#16038=PLANE('',#18950);
#16039=PLANE('',#18951);
#16040=PLANE('',#18952);
#16041=PLANE('',#18953);
#16042=PLANE('',#18954);
#16043=PLANE('',#18955);
#16044=PLANE('',#18956);
#16045=PLANE('',#18957);
#16046=PLANE('',#18958);
#16047=PLANE('',#18959);
#16048=PLANE('',#18960);
#16049=PLANE('',#18961);
#16050=PLANE('',#18962);
#16051=PLANE('',#18963);
#16052=PLANE('',#18964);
#16053=PLANE('',#18965);
#16054=PLANE('',#18966);
#16055=PLANE('',#18967);
#16056=PLANE('',#18968);
#16057=PLANE('',#18969);
#16058=PLANE('',#18970);
#16059=PLANE('',#18971);
#16060=PLANE('',#18972);
#16061=PLANE('',#18973);
#16062=PLANE('',#18974);
#16063=PLANE('',#18975);
#16064=PLANE('',#18976);
#16065=PLANE('',#18977);
#16066=PLANE('',#18978);
#16067=PLANE('',#18979);
#16068=PLANE('',#18980);
#16069=PLANE('',#18981);
#16070=PLANE('',#18982);
#16071=PLANE('',#18983);
#16072=PLANE('',#18984);
#16073=PLANE('',#18985);
#16074=PLANE('',#18986);
#16075=PLANE('',#18987);
#16076=PLANE('',#18988);
#16077=PLANE('',#18989);
#16078=PLANE('',#18990);
#16079=PLANE('',#18991);
#16080=PLANE('',#18992);
#16081=PLANE('',#18993);
#16082=PLANE('',#18994);
#16083=PLANE('',#18995);
#16084=PLANE('',#18996);
#16085=PLANE('',#18997);
#16086=PLANE('',#18998);
#16087=PLANE('',#19003);
#16088=PLANE('',#19008);
#16089=ADVANCED_FACE('',(#2280),#15615,.T.);
#16090=ADVANCED_FACE('',(#2281),#15616,.T.);
#16091=ADVANCED_FACE('',(#2282),#15617,.T.);
#16092=ADVANCED_FACE('',(#2283),#15618,.T.);
#16093=ADVANCED_FACE('',(#2284),#15619,.F.);
#16094=ADVANCED_FACE('',(#2285),#15620,.F.);
#16095=ADVANCED_FACE('',(#2286,#1432,#1433,#1434,#1435),#15621,.T.);
#16096=ADVANCED_FACE('',(#2287),#15622,.T.);
#16097=ADVANCED_FACE('',(#2288),#15623,.T.);
#16098=ADVANCED_FACE('',(#2289),#15624,.T.);
#16099=ADVANCED_FACE('',(#2290),#15625,.F.);
#16100=ADVANCED_FACE('',(#2291),#15626,.F.);
#16101=ADVANCED_FACE('',(#2292),#15627,.F.);
#16102=ADVANCED_FACE('',(#2293),#15628,.T.);
#16103=ADVANCED_FACE('',(#2294),#15629,.F.);
#16104=ADVANCED_FACE('',(#2295),#15630,.T.);
#16105=ADVANCED_FACE('',(#2296),#15631,.F.);
#16106=ADVANCED_FACE('',(#2297),#15632,.T.);
#16107=ADVANCED_FACE('',(#2298),#15633,.F.);
#16108=ADVANCED_FACE('',(#2299),#15634,.T.);
#16109=ADVANCED_FACE('',(#2300),#15635,.F.);
#16110=ADVANCED_FACE('',(#2301),#15636,.T.);
#16111=ADVANCED_FACE('',(#2302),#15637,.T.);
#16112=ADVANCED_FACE('',(#2303),#15638,.T.);
#16113=ADVANCED_FACE('',(#2304),#15639,.T.);
#16114=ADVANCED_FACE('',(#2305),#15640,.T.);
#16115=ADVANCED_FACE('',(#2306),#15641,.T.);
#16116=ADVANCED_FACE('',(#2307),#15642,.T.);
#16117=ADVANCED_FACE('',(#2308),#15643,.T.);
#16118=ADVANCED_FACE('',(#2309),#15644,.T.);
#16119=ADVANCED_FACE('',(#2310),#847,.T.);
#16120=ADVANCED_FACE('',(#2311),#139,.F.);
#16121=ADVANCED_FACE('',(#2312,#1436,#1437),#15645,.F.);
#16122=ADVANCED_FACE('',(#2313),#848,.T.);
#16123=ADVANCED_FACE('',(#2314),#15646,.T.);
#16124=ADVANCED_FACE('',(#2315),#15647,.F.);
#16125=ADVANCED_FACE('',(#2316),#15648,.T.);
#16126=ADVANCED_FACE('',(#2317),#15649,.F.);
#16127=ADVANCED_FACE('',(#2318),#15650,.T.);
#16128=ADVANCED_FACE('',(#2319),#15651,.F.);
#16129=ADVANCED_FACE('',(#2320),#15652,.T.);
#16130=ADVANCED_FACE('',(#2321),#15653,.F.);
#16131=ADVANCED_FACE('',(#2322),#15654,.T.);
#16132=ADVANCED_FACE('',(#2323),#15655,.F.);
#16133=ADVANCED_FACE('',(#2324),#849,.F.);
#16134=ADVANCED_FACE('',(#2325),#140,.F.);
#16135=ADVANCED_FACE('',(#2326),#15656,.T.);
#16136=ADVANCED_FACE('',(#2327),#15657,.T.);
#16137=ADVANCED_FACE('',(#2328),#15658,.T.);
#16138=ADVANCED_FACE('',(#2329),#15659,.T.);
#16139=ADVANCED_FACE('',(#2330),#15660,.T.);
#16140=ADVANCED_FACE('',(#2331,#1438),#15661,.T.);
#16141=ADVANCED_FACE('',(#2332),#850,.T.);
#16142=ADVANCED_FACE('',(#2333),#851,.T.);
#16143=ADVANCED_FACE('',(#2334),#141,.T.);
#16144=ADVANCED_FACE('',(#2335),#852,.F.);
#16145=ADVANCED_FACE('',(#2336),#142,.F.);
#16146=ADVANCED_FACE('',(#2337),#853,.T.);
#16147=ADVANCED_FACE('',(#2338,#1439,#1440,#1441),#15662,.T.);
#16148=ADVANCED_FACE('',(#2339),#854,.F.);
#16149=ADVANCED_FACE('',(#2340),#143,.F.);
#16150=ADVANCED_FACE('',(#2341),#15663,.T.);
#16151=ADVANCED_FACE('',(#2342,#1442),#15664,.F.);
#16152=ADVANCED_FACE('',(#2343),#144,.F.);
#16153=ADVANCED_FACE('',(#2344),#145,.F.);
#16154=ADVANCED_FACE('',(#2345),#15665,.T.);
#16155=ADVANCED_FACE('',(#2346),#15666,.F.);
#16156=ADVANCED_FACE('',(#2347),#15667,.F.);
#16157=ADVANCED_FACE('',(#2348),#15668,.F.);
#16158=ADVANCED_FACE('',(#2349),#15669,.F.);
#16159=ADVANCED_FACE('',(#2350),#15670,.F.);
#16160=ADVANCED_FACE('',(#2351),#15671,.F.);
#16161=ADVANCED_FACE('',(#2352),#15672,.T.);
#16162=ADVANCED_FACE('',(#2353),#146,.T.);
#16163=ADVANCED_FACE('',(#2354),#855,.T.);
#16164=ADVANCED_FACE('',(#2355),#15673,.T.);
#16165=ADVANCED_FACE('',(#2356),#147,.T.);
#16166=ADVANCED_FACE('',(#2357),#856,.T.);
#16167=ADVANCED_FACE('',(#2358),#15674,.T.);
#16168=ADVANCED_FACE('',(#2359),#148,.F.);
#16169=ADVANCED_FACE('',(#2360),#15675,.T.);
#16170=ADVANCED_FACE('',(#2361),#857,.F.);
#16171=ADVANCED_FACE('',(#2362),#149,.F.);
#16172=ADVANCED_FACE('',(#2363),#15676,.T.);
#16173=ADVANCED_FACE('',(#2364),#150,.F.);
#16174=ADVANCED_FACE('',(#2365),#858,.F.);
#16175=ADVANCED_FACE('',(#2366),#15677,.T.);
#16176=ADVANCED_FACE('',(#2367),#859,.F.);
#16177=ADVANCED_FACE('',(#2368),#151,.F.);
#16178=ADVANCED_FACE('',(#2369),#15678,.T.);
#16179=ADVANCED_FACE('',(#2370),#15679,.T.);
#16180=ADVANCED_FACE('',(#2371),#15680,.T.);
#16181=ADVANCED_FACE('',(#2372),#152,.F.);
#16182=ADVANCED_FACE('',(#2373),#860,.T.);
#16183=ADVANCED_FACE('',(#2374),#15681,.T.);
#16184=ADVANCED_FACE('',(#2375),#153,.T.);
#16185=ADVANCED_FACE('',(#2376),#861,.T.);
#16186=ADVANCED_FACE('',(#2377),#15682,.T.);
#16187=ADVANCED_FACE('',(#2378),#862,.T.);
#16188=ADVANCED_FACE('',(#2379),#154,.T.);
#16189=ADVANCED_FACE('',(#2380),#15683,.T.);
#16190=ADVANCED_FACE('',(#2381),#15684,.T.);
#16191=ADVANCED_FACE('',(#2382),#863,.T.);
#16192=ADVANCED_FACE('',(#2383),#155,.T.);
#16193=ADVANCED_FACE('',(#2384),#15685,.T.);
#16194=ADVANCED_FACE('',(#2385),#15686,.T.);
#16195=ADVANCED_FACE('',(#2386),#864,.T.);
#16196=ADVANCED_FACE('',(#2387),#156,.T.);
#16197=ADVANCED_FACE('',(#2388),#15687,.T.);
#16198=ADVANCED_FACE('',(#2389),#15688,.T.);
#16199=ADVANCED_FACE('',(#2390),#865,.T.);
#16200=ADVANCED_FACE('',(#2391),#157,.T.);
#16201=ADVANCED_FACE('',(#2392),#15689,.T.);
#16202=ADVANCED_FACE('',(#2393),#15690,.T.);
#16203=ADVANCED_FACE('',(#2394),#866,.T.);
#16204=ADVANCED_FACE('',(#2395),#158,.T.);
#16205=ADVANCED_FACE('',(#2396),#15691,.T.);
#16206=ADVANCED_FACE('',(#2397),#15692,.T.);
#16207=ADVANCED_FACE('',(#2398),#867,.T.);
#16208=ADVANCED_FACE('',(#2399),#159,.T.);
#16209=ADVANCED_FACE('',(#2400),#15693,.T.);
#16210=ADVANCED_FACE('',(#2401),#15694,.T.);
#16211=ADVANCED_FACE('',(#2402),#868,.T.);
#16212=ADVANCED_FACE('',(#2403),#160,.T.);
#16213=ADVANCED_FACE('',(#2404),#15695,.T.);
#16214=ADVANCED_FACE('',(#2405),#15696,.T.);
#16215=ADVANCED_FACE('',(#2406),#869,.T.);
#16216=ADVANCED_FACE('',(#2407),#161,.T.);
#16217=ADVANCED_FACE('',(#2408),#15697,.T.);
#16218=ADVANCED_FACE('',(#2409),#870,.F.);
#16219=ADVANCED_FACE('',(#2410),#871,.T.);
#16220=ADVANCED_FACE('',(#2411),#872,.T.);
#16221=ADVANCED_FACE('',(#2412),#873,.T.);
#16222=ADVANCED_FACE('',(#2413,#1443),#15698,.F.);
#16223=ADVANCED_FACE('',(#2414),#162,.F.);
#16224=ADVANCED_FACE('',(#2415),#15699,.T.);
#16225=ADVANCED_FACE('',(#2416),#15700,.T.);
#16226=ADVANCED_FACE('',(#2417),#874,.F.);
#16227=ADVANCED_FACE('',(#2418),#163,.F.);
#16228=ADVANCED_FACE('',(#2419),#15701,.T.);
#16229=ADVANCED_FACE('',(#2420),#15702,.T.);
#16230=ADVANCED_FACE('',(#2421),#875,.F.);
#16231=ADVANCED_FACE('',(#2422),#164,.F.);
#16232=ADVANCED_FACE('',(#2423),#15703,.T.);
#16233=ADVANCED_FACE('',(#2424),#15704,.T.);
#16234=ADVANCED_FACE('',(#2425),#876,.F.);
#16235=ADVANCED_FACE('',(#2426),#165,.F.);
#16236=ADVANCED_FACE('',(#2427),#15705,.T.);
#16237=ADVANCED_FACE('',(#2428),#166,.T.);
#16238=ADVANCED_FACE('',(#2429),#877,.T.);
#16239=ADVANCED_FACE('',(#2430),#15706,.T.);
#16240=ADVANCED_FACE('',(#2431),#15707,.T.);
#16241=ADVANCED_FACE('',(#2432),#878,.T.);
#16242=ADVANCED_FACE('',(#2433),#167,.T.);
#16243=ADVANCED_FACE('',(#2434),#15708,.T.);
#16244=ADVANCED_FACE('',(#2435),#15709,.T.);
#16245=ADVANCED_FACE('',(#2436),#879,.T.);
#16246=ADVANCED_FACE('',(#2437),#168,.T.);
#16247=ADVANCED_FACE('',(#2438),#15710,.T.);
#16248=ADVANCED_FACE('',(#2439),#15711,.T.);
#16249=ADVANCED_FACE('',(#2440),#880,.T.);
#16250=ADVANCED_FACE('',(#2441),#169,.T.);
#16251=ADVANCED_FACE('',(#2442),#15712,.T.);
#16252=ADVANCED_FACE('',(#2443),#15713,.T.);
#16253=ADVANCED_FACE('',(#2444),#881,.T.);
#16254=ADVANCED_FACE('',(#2445),#170,.T.);
#16255=ADVANCED_FACE('',(#2446),#15714,.T.);
#16256=ADVANCED_FACE('',(#2447),#15715,.T.);
#16257=ADVANCED_FACE('',(#2448),#882,.T.);
#16258=ADVANCED_FACE('',(#2449),#171,.T.);
#16259=ADVANCED_FACE('',(#2450),#15716,.T.);
#16260=ADVANCED_FACE('',(#2451),#15717,.T.);
#16261=ADVANCED_FACE('',(#2452),#883,.T.);
#16262=ADVANCED_FACE('',(#2453),#172,.T.);
#16263=ADVANCED_FACE('',(#2454),#15718,.T.);
#16264=ADVANCED_FACE('',(#2455),#884,.T.);
#16265=ADVANCED_FACE('',(#2456),#885,.T.);
#16266=ADVANCED_FACE('',(#2457),#886,.T.);
#16267=ADVANCED_FACE('',(#2458),#173,.T.);
#16268=ADVANCED_FACE('',(#2459),#174,.T.);
#16269=ADVANCED_FACE('',(#2460),#175,.T.);
#16270=ADVANCED_FACE('',(#2461),#15719,.T.);
#16271=ADVANCED_FACE('',(#2462),#887,.F.);
#16272=ADVANCED_FACE('',(#2463),#888,.F.);
#16273=ADVANCED_FACE('',(#2464),#889,.F.);
#16274=ADVANCED_FACE('',(#2465),#890,.F.);
#16275=ADVANCED_FACE('',(#2466),#891,.F.);
#16276=ADVANCED_FACE('',(#2467),#176,.F.);
#16277=ADVANCED_FACE('',(#2468),#177,.F.);
#16278=ADVANCED_FACE('',(#2469),#178,.F.);
#16279=ADVANCED_FACE('',(#2470),#179,.F.);
#16280=ADVANCED_FACE('',(#2471),#180,.F.);
#16281=ADVANCED_FACE('',(#2472),#181,.F.);
#16282=ADVANCED_FACE('',(#2473),#15720,.T.);
#16283=ADVANCED_FACE('',(#2474),#892,.F.);
#16284=ADVANCED_FACE('',(#2475),#182,.F.);
#16285=ADVANCED_FACE('',(#2476),#15721,.T.);
#16286=ADVANCED_FACE('',(#2477),#893,.T.);
#16287=ADVANCED_FACE('',(#2478),#15722,.T.);
#16288=ADVANCED_FACE('',(#2479),#894,.F.);
#16289=ADVANCED_FACE('',(#2480),#183,.F.);
#16290=ADVANCED_FACE('',(#2481),#15723,.T.);
#16291=ADVANCED_FACE('',(#2482),#15724,.T.);
#16292=ADVANCED_FACE('',(#2483),#895,.F.);
#16293=ADVANCED_FACE('',(#2484),#184,.F.);
#16294=ADVANCED_FACE('',(#2485),#15725,.T.);
#16295=ADVANCED_FACE('',(#2486),#15726,.T.);
#16296=ADVANCED_FACE('',(#2487),#896,.F.);
#16297=ADVANCED_FACE('',(#2488),#185,.F.);
#16298=ADVANCED_FACE('',(#2489),#15727,.T.);
#16299=ADVANCED_FACE('',(#2490),#186,.T.);
#16300=ADVANCED_FACE('',(#2491),#897,.T.);
#16301=ADVANCED_FACE('',(#2492),#15728,.T.);
#16302=ADVANCED_FACE('',(#2493),#15729,.T.);
#16303=ADVANCED_FACE('',(#2494),#898,.T.);
#16304=ADVANCED_FACE('',(#2495),#187,.T.);
#16305=ADVANCED_FACE('',(#2496),#15730,.T.);
#16306=ADVANCED_FACE('',(#2497),#15731,.T.);
#16307=ADVANCED_FACE('',(#2498),#899,.T.);
#16308=ADVANCED_FACE('',(#2499),#188,.T.);
#16309=ADVANCED_FACE('',(#2500),#15732,.T.);
#16310=ADVANCED_FACE('',(#2501),#15733,.T.);
#16311=ADVANCED_FACE('',(#2502),#900,.T.);
#16312=ADVANCED_FACE('',(#2503),#189,.T.);
#16313=ADVANCED_FACE('',(#2504),#15734,.T.);
#16314=ADVANCED_FACE('',(#2505),#15735,.T.);
#16315=ADVANCED_FACE('',(#2506),#901,.T.);
#16316=ADVANCED_FACE('',(#2507),#190,.T.);
#16317=ADVANCED_FACE('',(#2508),#15736,.T.);
#16318=ADVANCED_FACE('',(#2509),#15737,.T.);
#16319=ADVANCED_FACE('',(#2510),#902,.T.);
#16320=ADVANCED_FACE('',(#2511),#191,.T.);
#16321=ADVANCED_FACE('',(#2512),#15738,.T.);
#16322=ADVANCED_FACE('',(#2513),#903,.T.);
#16323=ADVANCED_FACE('',(#2514),#904,.T.);
#16324=ADVANCED_FACE('',(#2515),#905,.T.);
#16325=ADVANCED_FACE('',(#2516),#192,.T.);
#16326=ADVANCED_FACE('',(#2517),#193,.T.);
#16327=ADVANCED_FACE('',(#2518),#194,.T.);
#16328=ADVANCED_FACE('',(#2519),#195,.T.);
#16329=ADVANCED_FACE('',(#2520),#15739,.T.);
#16330=ADVANCED_FACE('',(#2521),#906,.F.);
#16331=ADVANCED_FACE('',(#2522),#907,.F.);
#16332=ADVANCED_FACE('',(#2523),#908,.F.);
#16333=ADVANCED_FACE('',(#2524),#909,.F.);
#16334=ADVANCED_FACE('',(#2525),#196,.F.);
#16335=ADVANCED_FACE('',(#2526),#197,.F.);
#16336=ADVANCED_FACE('',(#2527),#198,.F.);
#16337=ADVANCED_FACE('',(#2528),#199,.F.);
#16338=ADVANCED_FACE('',(#2529),#200,.F.);
#16339=ADVANCED_FACE('',(#2530),#15740,.T.);
#16340=ADVANCED_FACE('',(#2531),#910,.F.);
#16341=ADVANCED_FACE('',(#2532),#201,.F.);
#16342=ADVANCED_FACE('',(#2533),#15741,.T.);
#16343=ADVANCED_FACE('',(#2534),#15742,.T.);
#16344=ADVANCED_FACE('',(#2535),#911,.F.);
#16345=ADVANCED_FACE('',(#2536),#202,.F.);
#16346=ADVANCED_FACE('',(#2537),#15743,.T.);
#16347=ADVANCED_FACE('',(#2538),#15744,.T.);
#16348=ADVANCED_FACE('',(#2539),#912,.F.);
#16349=ADVANCED_FACE('',(#2540),#203,.F.);
#16350=ADVANCED_FACE('',(#2541),#15745,.T.);
#16351=ADVANCED_FACE('',(#2542),#15746,.T.);
#16352=ADVANCED_FACE('',(#2543),#913,.F.);
#16353=ADVANCED_FACE('',(#2544),#204,.F.);
#16354=ADVANCED_FACE('',(#2545),#15747,.T.);
#16355=ADVANCED_FACE('',(#2546),#15748,.T.);
#16356=ADVANCED_FACE('',(#2547),#914,.F.);
#16357=ADVANCED_FACE('',(#2548),#205,.F.);
#16358=ADVANCED_FACE('',(#2549),#15749,.T.);
#16359=ADVANCED_FACE('',(#2550),#206,.T.);
#16360=ADVANCED_FACE('',(#2551),#915,.T.);
#16361=ADVANCED_FACE('',(#2552),#15750,.T.);
#16362=ADVANCED_FACE('',(#2553),#15751,.T.);
#16363=ADVANCED_FACE('',(#2554),#916,.T.);
#16364=ADVANCED_FACE('',(#2555),#207,.T.);
#16365=ADVANCED_FACE('',(#2556),#15752,.T.);
#16366=ADVANCED_FACE('',(#2557),#15753,.T.);
#16367=ADVANCED_FACE('',(#2558),#917,.T.);
#16368=ADVANCED_FACE('',(#2559),#208,.T.);
#16369=ADVANCED_FACE('',(#2560),#15754,.T.);
#16370=ADVANCED_FACE('',(#2561),#15755,.T.);
#16371=ADVANCED_FACE('',(#2562),#918,.T.);
#16372=ADVANCED_FACE('',(#2563),#209,.T.);
#16373=ADVANCED_FACE('',(#2564),#15756,.T.);
#16374=ADVANCED_FACE('',(#2565),#15757,.T.);
#16375=ADVANCED_FACE('',(#2566),#919,.T.);
#16376=ADVANCED_FACE('',(#2567),#210,.T.);
#16377=ADVANCED_FACE('',(#2568),#15758,.T.);
#16378=ADVANCED_FACE('',(#2569),#920,.T.);
#16379=ADVANCED_FACE('',(#2570),#921,.T.);
#16380=ADVANCED_FACE('',(#2571),#922,.T.);
#16381=ADVANCED_FACE('',(#2572),#923,.T.);
#16382=ADVANCED_FACE('',(#2573),#924,.T.);
#16383=ADVANCED_FACE('',(#2574),#211,.T.);
#16384=ADVANCED_FACE('',(#2575),#212,.T.);
#16385=ADVANCED_FACE('',(#2576),#213,.T.);
#16386=ADVANCED_FACE('',(#2577),#214,.T.);
#16387=ADVANCED_FACE('',(#2578),#215,.T.);
#16388=ADVANCED_FACE('',(#2579),#15759,.T.);
#16389=ADVANCED_FACE('',(#2580),#925,.F.);
#16390=ADVANCED_FACE('',(#2581),#926,.F.);
#16391=ADVANCED_FACE('',(#2582),#927,.F.);
#16392=ADVANCED_FACE('',(#2583),#216,.F.);
#16393=ADVANCED_FACE('',(#2584),#217,.F.);
#16394=ADVANCED_FACE('',(#2585),#218,.F.);
#16395=ADVANCED_FACE('',(#2586),#219,.F.);
#16396=ADVANCED_FACE('',(#2587),#15760,.T.);
#16397=ADVANCED_FACE('',(#2588),#928,.F.);
#16398=ADVANCED_FACE('',(#2589),#220,.F.);
#16399=ADVANCED_FACE('',(#2590),#15761,.T.);
#16400=ADVANCED_FACE('',(#2591),#929,.T.);
#16401=ADVANCED_FACE('',(#2592),#15762,.T.);
#16402=ADVANCED_FACE('',(#2593),#930,.F.);
#16403=ADVANCED_FACE('',(#2594),#221,.F.);
#16404=ADVANCED_FACE('',(#2595),#15763,.T.);
#16405=ADVANCED_FACE('',(#2596),#15764,.T.);
#16406=ADVANCED_FACE('',(#2597),#931,.F.);
#16407=ADVANCED_FACE('',(#2598),#222,.F.);
#16408=ADVANCED_FACE('',(#2599),#15765,.T.);
#16409=ADVANCED_FACE('',(#2600),#15766,.T.);
#16410=ADVANCED_FACE('',(#2601),#932,.F.);
#16411=ADVANCED_FACE('',(#2602),#223,.F.);
#16412=ADVANCED_FACE('',(#2603),#15767,.T.);
#16413=ADVANCED_FACE('',(#2604),#15768,.T.);
#16414=ADVANCED_FACE('',(#2605),#933,.F.);
#16415=ADVANCED_FACE('',(#2606),#224,.F.);
#16416=ADVANCED_FACE('',(#2607),#15769,.T.);
#16417=ADVANCED_FACE('',(#2608),#15770,.T.);
#16418=ADVANCED_FACE('',(#2609),#934,.F.);
#16419=ADVANCED_FACE('',(#2610),#225,.F.);
#16420=ADVANCED_FACE('',(#2611),#15771,.T.);
#16421=ADVANCED_FACE('',(#2612),#226,.T.);
#16422=ADVANCED_FACE('',(#2613),#935,.T.);
#16423=ADVANCED_FACE('',(#2614),#15772,.T.);
#16424=ADVANCED_FACE('',(#2615),#15773,.T.);
#16425=ADVANCED_FACE('',(#2616),#936,.T.);
#16426=ADVANCED_FACE('',(#2617),#227,.T.);
#16427=ADVANCED_FACE('',(#2618),#15774,.T.);
#16428=ADVANCED_FACE('',(#2619),#15775,.T.);
#16429=ADVANCED_FACE('',(#2620),#937,.T.);
#16430=ADVANCED_FACE('',(#2621),#228,.T.);
#16431=ADVANCED_FACE('',(#2622),#15776,.T.);
#16432=ADVANCED_FACE('',(#2623),#15777,.T.);
#16433=ADVANCED_FACE('',(#2624),#938,.T.);
#16434=ADVANCED_FACE('',(#2625),#229,.T.);
#16435=ADVANCED_FACE('',(#2626),#15778,.T.);
#16436=ADVANCED_FACE('',(#2627),#939,.T.);
#16437=ADVANCED_FACE('',(#2628),#940,.T.);
#16438=ADVANCED_FACE('',(#2629),#941,.T.);
#16439=ADVANCED_FACE('',(#2630),#942,.T.);
#16440=ADVANCED_FACE('',(#2631),#943,.T.);
#16441=ADVANCED_FACE('',(#2632),#230,.T.);
#16442=ADVANCED_FACE('',(#2633),#231,.T.);
#16443=ADVANCED_FACE('',(#2634),#232,.T.);
#16444=ADVANCED_FACE('',(#2635),#233,.T.);
#16445=ADVANCED_FACE('',(#2636),#234,.T.);
#16446=ADVANCED_FACE('',(#2637),#235,.T.);
#16447=ADVANCED_FACE('',(#2638),#15779,.T.);
#16448=ADVANCED_FACE('',(#2639),#944,.F.);
#16449=ADVANCED_FACE('',(#2640),#945,.F.);
#16450=ADVANCED_FACE('',(#2641),#236,.F.);
#16451=ADVANCED_FACE('',(#2642),#237,.F.);
#16452=ADVANCED_FACE('',(#2643),#238,.F.);
#16453=ADVANCED_FACE('',(#2644),#15780,.T.);
#16454=ADVANCED_FACE('',(#2645),#946,.F.);
#16455=ADVANCED_FACE('',(#2646),#239,.F.);
#16456=ADVANCED_FACE('',(#2647),#15781,.T.);
#16457=ADVANCED_FACE('',(#2648),#15782,.T.);
#16458=ADVANCED_FACE('',(#2649),#947,.F.);
#16459=ADVANCED_FACE('',(#2650),#240,.F.);
#16460=ADVANCED_FACE('',(#2651),#15783,.T.);
#16461=ADVANCED_FACE('',(#2652),#15784,.T.);
#16462=ADVANCED_FACE('',(#2653),#948,.F.);
#16463=ADVANCED_FACE('',(#2654),#241,.F.);
#16464=ADVANCED_FACE('',(#2655),#15785,.T.);
#16465=ADVANCED_FACE('',(#2656),#15786,.T.);
#16466=ADVANCED_FACE('',(#2657),#949,.F.);
#16467=ADVANCED_FACE('',(#2658),#242,.F.);
#16468=ADVANCED_FACE('',(#2659),#15787,.T.);
#16469=ADVANCED_FACE('',(#2660),#15788,.T.);
#16470=ADVANCED_FACE('',(#2661),#950,.F.);
#16471=ADVANCED_FACE('',(#2662),#243,.F.);
#16472=ADVANCED_FACE('',(#2663),#15789,.T.);
#16473=ADVANCED_FACE('',(#2664),#15790,.T.);
#16474=ADVANCED_FACE('',(#2665),#951,.F.);
#16475=ADVANCED_FACE('',(#2666),#244,.F.);
#16476=ADVANCED_FACE('',(#2667),#15791,.T.);
#16477=ADVANCED_FACE('',(#2668),#15792,.T.);
#16478=ADVANCED_FACE('',(#2669),#952,.F.);
#16479=ADVANCED_FACE('',(#2670),#245,.F.);
#16480=ADVANCED_FACE('',(#2671),#15793,.T.);
#16481=ADVANCED_FACE('',(#2672),#246,.T.);
#16482=ADVANCED_FACE('',(#2673),#953,.T.);
#16483=ADVANCED_FACE('',(#2674),#15794,.T.);
#16484=ADVANCED_FACE('',(#2675),#15795,.T.);
#16485=ADVANCED_FACE('',(#2676),#954,.T.);
#16486=ADVANCED_FACE('',(#2677),#247,.T.);
#16487=ADVANCED_FACE('',(#2678),#15796,.T.);
#16488=ADVANCED_FACE('',(#2679),#15797,.T.);
#16489=ADVANCED_FACE('',(#2680),#955,.T.);
#16490=ADVANCED_FACE('',(#2681),#248,.T.);
#16491=ADVANCED_FACE('',(#2682),#15798,.T.);
#16492=ADVANCED_FACE('',(#2683),#956,.T.);
#16493=ADVANCED_FACE('',(#2684),#957,.T.);
#16494=ADVANCED_FACE('',(#2685),#958,.T.);
#16495=ADVANCED_FACE('',(#2686),#959,.T.);
#16496=ADVANCED_FACE('',(#2687),#960,.T.);
#16497=ADVANCED_FACE('',(#2688),#961,.T.);
#16498=ADVANCED_FACE('',(#2689),#962,.T.);
#16499=ADVANCED_FACE('',(#2690),#249,.T.);
#16500=ADVANCED_FACE('',(#2691),#250,.T.);
#16501=ADVANCED_FACE('',(#2692),#251,.T.);
#16502=ADVANCED_FACE('',(#2693),#252,.T.);
#16503=ADVANCED_FACE('',(#2694),#253,.T.);
#16504=ADVANCED_FACE('',(#2695),#254,.T.);
#16505=ADVANCED_FACE('',(#2696),#255,.T.);
#16506=ADVANCED_FACE('',(#2697),#15799,.T.);
#16507=ADVANCED_FACE('',(#2698),#963,.F.);
#16508=ADVANCED_FACE('',(#2699),#256,.F.);
#16509=ADVANCED_FACE('',(#2700),#257,.F.);
#16510=ADVANCED_FACE('',(#2701),#15800,.T.);
#16511=ADVANCED_FACE('',(#2702),#964,.F.);
#16512=ADVANCED_FACE('',(#2703),#258,.F.);
#16513=ADVANCED_FACE('',(#2704),#15801,.T.);
#16514=ADVANCED_FACE('',(#2705),#15802,.T.);
#16515=ADVANCED_FACE('',(#2706),#965,.F.);
#16516=ADVANCED_FACE('',(#2707),#259,.F.);
#16517=ADVANCED_FACE('',(#2708),#15803,.T.);
#16518=ADVANCED_FACE('',(#2709),#15804,.T.);
#16519=ADVANCED_FACE('',(#2710),#966,.F.);
#16520=ADVANCED_FACE('',(#2711),#260,.F.);
#16521=ADVANCED_FACE('',(#2712),#15805,.T.);
#16522=ADVANCED_FACE('',(#2713),#15806,.T.);
#16523=ADVANCED_FACE('',(#2714),#967,.F.);
#16524=ADVANCED_FACE('',(#2715),#261,.F.);
#16525=ADVANCED_FACE('',(#2716),#15807,.T.);
#16526=ADVANCED_FACE('',(#2717),#15808,.T.);
#16527=ADVANCED_FACE('',(#2718),#968,.F.);
#16528=ADVANCED_FACE('',(#2719),#262,.F.);
#16529=ADVANCED_FACE('',(#2720),#15809,.T.);
#16530=ADVANCED_FACE('',(#2721),#15810,.T.);
#16531=ADVANCED_FACE('',(#2722),#969,.F.);
#16532=ADVANCED_FACE('',(#2723),#263,.F.);
#16533=ADVANCED_FACE('',(#2724),#15811,.T.);
#16534=ADVANCED_FACE('',(#2725),#15812,.T.);
#16535=ADVANCED_FACE('',(#2726),#970,.F.);
#16536=ADVANCED_FACE('',(#2727),#264,.F.);
#16537=ADVANCED_FACE('',(#2728),#15813,.T.);
#16538=ADVANCED_FACE('',(#2729),#15814,.T.);
#16539=ADVANCED_FACE('',(#2730),#971,.F.);
#16540=ADVANCED_FACE('',(#2731),#265,.F.);
#16541=ADVANCED_FACE('',(#2732),#15815,.T.);
#16542=ADVANCED_FACE('',(#2733),#266,.T.);
#16543=ADVANCED_FACE('',(#2734),#972,.T.);
#16544=ADVANCED_FACE('',(#2735),#15816,.T.);
#16545=ADVANCED_FACE('',(#2736),#15817,.T.);
#16546=ADVANCED_FACE('',(#2737),#973,.T.);
#16547=ADVANCED_FACE('',(#2738),#267,.T.);
#16548=ADVANCED_FACE('',(#2739),#15818,.T.);
#16549=ADVANCED_FACE('',(#2740),#974,.T.);
#16550=ADVANCED_FACE('',(#2741),#975,.T.);
#16551=ADVANCED_FACE('',(#2742),#976,.T.);
#16552=ADVANCED_FACE('',(#2743),#977,.T.);
#16553=ADVANCED_FACE('',(#2744),#978,.T.);
#16554=ADVANCED_FACE('',(#2745),#979,.T.);
#16555=ADVANCED_FACE('',(#2746),#980,.T.);
#16556=ADVANCED_FACE('',(#2747),#981,.T.);
#16557=ADVANCED_FACE('',(#2748),#268,.T.);
#16558=ADVANCED_FACE('',(#2749),#269,.T.);
#16559=ADVANCED_FACE('',(#2750),#270,.T.);
#16560=ADVANCED_FACE('',(#2751),#271,.T.);
#16561=ADVANCED_FACE('',(#2752),#272,.T.);
#16562=ADVANCED_FACE('',(#2753),#273,.T.);
#16563=ADVANCED_FACE('',(#2754),#274,.T.);
#16564=ADVANCED_FACE('',(#2755),#275,.T.);
#16565=ADVANCED_FACE('',(#2756),#15819,.T.);
#16566=ADVANCED_FACE('',(#2757),#276,.F.);
#16567=ADVANCED_FACE('',(#2758),#15820,.T.);
#16568=ADVANCED_FACE('',(#2759),#982,.T.);
#16569=ADVANCED_FACE('',(#2760),#277,.T.);
#16570=ADVANCED_FACE('',(#2761),#15821,.T.);
#16571=ADVANCED_FACE('',(#2762),#15822,.T.);
#16572=ADVANCED_FACE('',(#2763),#983,.T.);
#16573=ADVANCED_FACE('',(#2764),#278,.T.);
#16574=ADVANCED_FACE('',(#2765),#15823,.T.);
#16575=ADVANCED_FACE('',(#2766),#15824,.T.);
#16576=ADVANCED_FACE('',(#2767),#984,.T.);
#16577=ADVANCED_FACE('',(#2768),#279,.T.);
#16578=ADVANCED_FACE('',(#2769),#15825,.T.);
#16579=ADVANCED_FACE('',(#2770),#15826,.T.);
#16580=ADVANCED_FACE('',(#2771),#985,.T.);
#16581=ADVANCED_FACE('',(#2772),#280,.T.);
#16582=ADVANCED_FACE('',(#2773),#15827,.T.);
#16583=ADVANCED_FACE('',(#2774),#15828,.T.);
#16584=ADVANCED_FACE('',(#2775),#986,.T.);
#16585=ADVANCED_FACE('',(#2776),#281,.T.);
#16586=ADVANCED_FACE('',(#2777),#15829,.T.);
#16587=ADVANCED_FACE('',(#2778),#15830,.T.);
#16588=ADVANCED_FACE('',(#2779),#987,.T.);
#16589=ADVANCED_FACE('',(#2780),#282,.T.);
#16590=ADVANCED_FACE('',(#2781),#15831,.T.);
#16591=ADVANCED_FACE('',(#2782),#15832,.T.);
#16592=ADVANCED_FACE('',(#2783),#988,.T.);
#16593=ADVANCED_FACE('',(#2784),#283,.T.);
#16594=ADVANCED_FACE('',(#2785),#15833,.T.);
#16595=ADVANCED_FACE('',(#2786),#15834,.T.);
#16596=ADVANCED_FACE('',(#2787),#989,.T.);
#16597=ADVANCED_FACE('',(#2788),#284,.T.);
#16598=ADVANCED_FACE('',(#2789),#15835,.T.);
#16599=ADVANCED_FACE('',(#2790),#15836,.T.);
#16600=ADVANCED_FACE('',(#2791),#990,.T.);
#16601=ADVANCED_FACE('',(#2792),#285,.T.);
#16602=ADVANCED_FACE('',(#2793),#15837,.T.);
#16603=ADVANCED_FACE('',(#2794),#286,.F.);
#16604=ADVANCED_FACE('',(#2795),#991,.F.);
#16605=ADVANCED_FACE('',(#2796),#15838,.T.);
#16606=ADVANCED_FACE('',(#2797),#992,.F.);
#16607=ADVANCED_FACE('',(#2798),#993,.F.);
#16608=ADVANCED_FACE('',(#2799),#994,.F.);
#16609=ADVANCED_FACE('',(#2800),#995,.F.);
#16610=ADVANCED_FACE('',(#2801),#996,.F.);
#16611=ADVANCED_FACE('',(#2802),#997,.F.);
#16612=ADVANCED_FACE('',(#2803),#998,.F.);
#16613=ADVANCED_FACE('',(#2804),#999,.F.);
#16614=ADVANCED_FACE('',(#2805),#287,.F.);
#16615=ADVANCED_FACE('',(#2806),#288,.F.);
#16616=ADVANCED_FACE('',(#2807),#289,.F.);
#16617=ADVANCED_FACE('',(#2808),#290,.F.);
#16618=ADVANCED_FACE('',(#2809),#291,.F.);
#16619=ADVANCED_FACE('',(#2810),#292,.F.);
#16620=ADVANCED_FACE('',(#2811),#293,.F.);
#16621=ADVANCED_FACE('',(#2812),#294,.F.);
#16622=ADVANCED_FACE('',(#2813),#1000,.F.);
#16623=ADVANCED_FACE('',(#2814),#295,.F.);
#16624=ADVANCED_FACE('',(#2815),#15839,.T.);
#16625=ADVANCED_FACE('',(#2816),#1001,.F.);
#16626=ADVANCED_FACE('',(#2817),#1002,.F.);
#16627=ADVANCED_FACE('',(#2818),#1003,.F.);
#16628=ADVANCED_FACE('',(#2819),#1004,.F.);
#16629=ADVANCED_FACE('',(#2820),#1005,.F.);
#16630=ADVANCED_FACE('',(#2821),#1006,.F.);
#16631=ADVANCED_FACE('',(#2822),#1007,.F.);
#16632=ADVANCED_FACE('',(#2823),#1008,.F.);
#16633=ADVANCED_FACE('',(#2824),#296,.F.);
#16634=ADVANCED_FACE('',(#2825),#297,.F.);
#16635=ADVANCED_FACE('',(#2826),#298,.F.);
#16636=ADVANCED_FACE('',(#2827),#299,.F.);
#16637=ADVANCED_FACE('',(#2828),#300,.F.);
#16638=ADVANCED_FACE('',(#2829),#301,.F.);
#16639=ADVANCED_FACE('',(#2830),#302,.F.);
#16640=ADVANCED_FACE('',(#2831),#303,.F.);
#16641=ADVANCED_FACE('',(#2832),#304,.F.);
#16642=ADVANCED_FACE('',(#2833),#15840,.T.);
#16643=ADVANCED_FACE('',(#2834),#305,.F.);
#16644=ADVANCED_FACE('',(#2835),#15841,.T.);
#16645=ADVANCED_FACE('',(#2836),#1009,.T.);
#16646=ADVANCED_FACE('',(#2837),#15842,.T.);
#16647=ADVANCED_FACE('',(#2838),#306,.F.);
#16648=ADVANCED_FACE('',(#2839),#15843,.T.);
#16649=ADVANCED_FACE('',(#2840),#1010,.T.);
#16650=ADVANCED_FACE('',(#2841),#15844,.T.);
#16651=ADVANCED_FACE('',(#2842),#307,.F.);
#16652=ADVANCED_FACE('',(#2843),#15845,.T.);
#16653=ADVANCED_FACE('',(#2844),#1011,.T.);
#16654=ADVANCED_FACE('',(#2845),#15846,.T.);
#16655=ADVANCED_FACE('',(#2846),#308,.F.);
#16656=ADVANCED_FACE('',(#2847),#15847,.T.);
#16657=ADVANCED_FACE('',(#2848),#1012,.T.);
#16658=ADVANCED_FACE('',(#2849),#15848,.T.);
#16659=ADVANCED_FACE('',(#2850),#309,.F.);
#16660=ADVANCED_FACE('',(#2851),#15849,.T.);
#16661=ADVANCED_FACE('',(#2852),#1013,.T.);
#16662=ADVANCED_FACE('',(#2853),#15850,.T.);
#16663=ADVANCED_FACE('',(#2854),#310,.F.);
#16664=ADVANCED_FACE('',(#2855),#15851,.T.);
#16665=ADVANCED_FACE('',(#2856),#1014,.T.);
#16666=ADVANCED_FACE('',(#2857),#15852,.T.);
#16667=ADVANCED_FACE('',(#2858),#1015,.T.);
#16668=ADVANCED_FACE('',(#2859,#1444),#15853,.T.);
#16669=ADVANCED_FACE('',(#2860),#1016,.T.);
#16670=ADVANCED_FACE('',(#2861),#1017,.F.);
#16671=ADVANCED_FACE('',(#2862,#1445,#1446,#1447,#1448,#1449,#1450),#15854,
 .T.);
#16672=ADVANCED_FACE('',(#2863),#311,.F.);
#16673=ADVANCED_FACE('',(#2864),#1018,.F.);
#16674=ADVANCED_FACE('',(#2865),#312,.F.);
#16675=ADVANCED_FACE('',(#2866),#1019,.F.);
#16676=ADVANCED_FACE('',(#2867),#313,.F.);
#16677=ADVANCED_FACE('',(#2868),#1020,.F.);
#16678=ADVANCED_FACE('',(#2869),#314,.F.);
#16679=ADVANCED_FACE('',(#2870),#1021,.F.);
#16680=ADVANCED_FACE('',(#2871),#315,.F.);
#16681=ADVANCED_FACE('',(#2872),#1022,.F.);
#16682=ADVANCED_FACE('',(#2873),#316,.F.);
#16683=ADVANCED_FACE('',(#2874),#317,.T.);
#16684=ADVANCED_FACE('',(#2875),#318,.T.);
#16685=ADVANCED_FACE('',(#2876),#319,.T.);
#16686=ADVANCED_FACE('',(#2877),#320,.T.);
#16687=ADVANCED_FACE('',(#2878),#321,.T.);
#16688=ADVANCED_FACE('',(#2879),#322,.T.);
#16689=ADVANCED_FACE('',(#2880),#323,.T.);
#16690=ADVANCED_FACE('',(#2881),#324,.T.);
#16691=ADVANCED_FACE('',(#2882),#325,.T.);
#16692=ADVANCED_FACE('',(#2883),#326,.T.);
#16693=ADVANCED_FACE('',(#2884),#15855,.F.);
#16694=ADVANCED_FACE('',(#2885),#15856,.F.);
#16695=ADVANCED_FACE('',(#2886),#15857,.F.);
#16696=ADVANCED_FACE('',(#2887),#15858,.F.);
#16697=ADVANCED_FACE('',(#2888),#15859,.F.);
#16698=ADVANCED_FACE('',(#2889),#15860,.F.);
#16699=ADVANCED_FACE('',(#2890),#327,.F.);
#16700=ADVANCED_FACE('',(#2891),#15861,.F.);
#16701=ADVANCED_FACE('',(#2892),#15862,.F.);
#16702=ADVANCED_FACE('',(#2893),#15863,.F.);
#16703=ADVANCED_FACE('',(#2894),#15864,.F.);
#16704=ADVANCED_FACE('',(#2895),#15865,.F.);
#16705=ADVANCED_FACE('',(#2896),#15866,.F.);
#16706=ADVANCED_FACE('',(#2897),#15867,.F.);
#16707=ADVANCED_FACE('',(#2898),#15868,.F.);
#16708=ADVANCED_FACE('',(#2899),#15869,.F.);
#16709=ADVANCED_FACE('',(#2900),#15870,.F.);
#16710=ADVANCED_FACE('',(#2901),#328,.F.);
#16711=ADVANCED_FACE('',(#2902),#15871,.F.);
#16712=ADVANCED_FACE('',(#2903),#15872,.F.);
#16713=ADVANCED_FACE('',(#2904),#15873,.F.);
#16714=ADVANCED_FACE('',(#2905),#15874,.F.);
#16715=ADVANCED_FACE('',(#2906),#15875,.F.);
#16716=ADVANCED_FACE('',(#2907),#15876,.F.);
#16717=ADVANCED_FACE('',(#2908),#15877,.F.);
#16718=ADVANCED_FACE('',(#2909),#15878,.F.);
#16719=ADVANCED_FACE('',(#2910),#15879,.F.);
#16720=ADVANCED_FACE('',(#2911),#15880,.F.);
#16721=ADVANCED_FACE('',(#2912),#329,.F.);
#16722=ADVANCED_FACE('',(#2913),#15881,.F.);
#16723=ADVANCED_FACE('',(#2914),#15882,.F.);
#16724=ADVANCED_FACE('',(#2915),#15883,.F.);
#16725=ADVANCED_FACE('',(#2916),#15884,.F.);
#16726=ADVANCED_FACE('',(#2917),#15885,.F.);
#16727=ADVANCED_FACE('',(#2918),#15886,.F.);
#16728=ADVANCED_FACE('',(#2919),#15887,.F.);
#16729=ADVANCED_FACE('',(#2920),#15888,.F.);
#16730=ADVANCED_FACE('',(#2921),#15889,.F.);
#16731=ADVANCED_FACE('',(#2922),#15890,.F.);
#16732=ADVANCED_FACE('',(#2923),#15891,.F.);
#16733=ADVANCED_FACE('',(#2924),#15892,.F.);
#16734=ADVANCED_FACE('',(#2925),#15893,.F.);
#16735=ADVANCED_FACE('',(#2926),#15894,.F.);
#16736=ADVANCED_FACE('',(#2927),#15895,.F.);
#16737=ADVANCED_FACE('',(#2928),#15896,.F.);
#16738=ADVANCED_FACE('',(#2929),#15897,.F.);
#16739=ADVANCED_FACE('',(#2930),#15898,.F.);
#16740=ADVANCED_FACE('',(#2931),#15899,.F.);
#16741=ADVANCED_FACE('',(#2932),#15900,.F.);
#16742=ADVANCED_FACE('',(#2933),#15901,.F.);
#16743=ADVANCED_FACE('',(#2934),#15902,.F.);
#16744=ADVANCED_FACE('',(#2935),#15903,.F.);
#16745=ADVANCED_FACE('',(#2936),#15904,.F.);
#16746=ADVANCED_FACE('',(#2937),#15905,.F.);
#16747=ADVANCED_FACE('',(#2938),#15906,.F.);
#16748=ADVANCED_FACE('',(#2939),#15907,.F.);
#16749=ADVANCED_FACE('',(#2940),#15908,.F.);
#16750=ADVANCED_FACE('',(#2941),#15909,.F.);
#16751=ADVANCED_FACE('',(#2942),#15910,.F.);
#16752=ADVANCED_FACE('',(#2943),#15911,.F.);
#16753=ADVANCED_FACE('',(#2944),#15912,.F.);
#16754=ADVANCED_FACE('',(#2945),#15913,.F.);
#16755=ADVANCED_FACE('',(#2946),#15914,.F.);
#16756=ADVANCED_FACE('',(#2947),#15915,.F.);
#16757=ADVANCED_FACE('',(#2948),#15916,.F.);
#16758=ADVANCED_FACE('',(#2949),#15917,.F.);
#16759=ADVANCED_FACE('',(#2950),#15918,.F.);
#16760=ADVANCED_FACE('',(#2951),#15919,.F.);
#16761=ADVANCED_FACE('',(#2952),#15920,.F.);
#16762=ADVANCED_FACE('',(#2953),#15921,.F.);
#16763=ADVANCED_FACE('',(#2954),#330,.F.);
#16764=ADVANCED_FACE('',(#2955),#15922,.F.);
#16765=ADVANCED_FACE('',(#2956),#15923,.F.);
#16766=ADVANCED_FACE('',(#2957),#15924,.F.);
#16767=ADVANCED_FACE('',(#2958),#15925,.F.);
#16768=ADVANCED_FACE('',(#2959),#15926,.F.);
#16769=ADVANCED_FACE('',(#2960),#15927,.F.);
#16770=ADVANCED_FACE('',(#2961),#15928,.F.);
#16771=ADVANCED_FACE('',(#2962),#15929,.F.);
#16772=ADVANCED_FACE('',(#2963),#15930,.F.);
#16773=ADVANCED_FACE('',(#2964),#331,.F.);
#16774=ADVANCED_FACE('',(#2965),#15931,.F.);
#16775=ADVANCED_FACE('',(#2966),#15932,.F.);
#16776=ADVANCED_FACE('',(#2967),#15933,.F.);
#16777=ADVANCED_FACE('',(#2968),#15934,.F.);
#16778=ADVANCED_FACE('',(#2969),#15935,.F.);
#16779=ADVANCED_FACE('',(#2970),#15936,.F.);
#16780=ADVANCED_FACE('',(#2971),#15937,.F.);
#16781=ADVANCED_FACE('',(#2972),#15938,.F.);
#16782=ADVANCED_FACE('',(#2973),#15939,.F.);
#16783=ADVANCED_FACE('',(#2974),#15940,.F.);
#16784=ADVANCED_FACE('',(#2975),#332,.F.);
#16785=ADVANCED_FACE('',(#2976),#15941,.F.);
#16786=ADVANCED_FACE('',(#2977),#15942,.F.);
#16787=ADVANCED_FACE('',(#2978),#15943,.F.);
#16788=ADVANCED_FACE('',(#2979),#15944,.F.);
#16789=ADVANCED_FACE('',(#2980),#1023,.F.);
#16790=ADVANCED_FACE('',(#2981),#1024,.F.);
#16791=ADVANCED_FACE('',(#2982),#1025,.F.);
#16792=ADVANCED_FACE('',(#2983),#1026,.F.);
#16793=ADVANCED_FACE('',(#2984),#1027,.F.);
#16794=ADVANCED_FACE('',(#2985),#333,.F.);
#16795=ADVANCED_FACE('',(#2986,#1451,#1452,#1453,#1454,#1455,#1456,#1457,
#1458,#1459,#1460,#1461),#15945,.F.);
#16796=ADVANCED_FACE('',(#2987),#334,.F.);
#16797=ADVANCED_FACE('',(#2988),#335,.F.);
#16798=ADVANCED_FACE('',(#2989),#336,.F.);
#16799=ADVANCED_FACE('',(#2990),#337,.F.);
#16800=ADVANCED_FACE('',(#2991),#338,.F.);
#16801=ADVANCED_FACE('',(#2992),#339,.F.);
#16802=ADVANCED_FACE('',(#2993),#340,.F.);
#16803=ADVANCED_FACE('',(#2994),#341,.F.);
#16804=ADVANCED_FACE('',(#2995),#342,.F.);
#16805=ADVANCED_FACE('',(#2996),#343,.F.);
#16806=ADVANCED_FACE('',(#2997),#344,.F.);
#16807=ADVANCED_FACE('',(#2998),#345,.F.);
#16808=ADVANCED_FACE('',(#2999),#346,.F.);
#16809=ADVANCED_FACE('',(#3000),#347,.F.);
#16810=ADVANCED_FACE('',(#3001),#348,.F.);
#16811=ADVANCED_FACE('',(#3002),#349,.F.);
#16812=ADVANCED_FACE('',(#3003),#350,.F.);
#16813=ADVANCED_FACE('',(#3004),#351,.F.);
#16814=ADVANCED_FACE('',(#3005),#352,.F.);
#16815=ADVANCED_FACE('',(#3006),#353,.F.);
#16816=ADVANCED_FACE('',(#3007),#354,.F.);
#16817=ADVANCED_FACE('',(#3008),#355,.F.);
#16818=ADVANCED_FACE('',(#3009),#356,.F.);
#16819=ADVANCED_FACE('',(#3010),#357,.F.);
#16820=ADVANCED_FACE('',(#3011),#358,.F.);
#16821=ADVANCED_FACE('',(#3012),#76,.F.);
#16822=ADVANCED_FACE('',(#3013),#77,.F.);
#16823=ADVANCED_FACE('',(#3014,#1462),#15946,.T.);
#16824=ADVANCED_FACE('',(#3015),#359,.F.);
#16825=ADVANCED_FACE('',(#3016),#360,.T.);
#16826=ADVANCED_FACE('',(#3017,#1463),#15947,.T.);
#16827=ADVANCED_FACE('',(#3018),#361,.T.);
#16828=ADVANCED_FACE('',(#3019),#1028,.T.);
#16829=ADVANCED_FACE('',(#3020,#1464),#15948,.T.);
#16830=ADVANCED_FACE('',(#3021),#362,.T.);
#16831=ADVANCED_FACE('',(#3022),#363,.T.);
#16832=ADVANCED_FACE('',(#3023),#364,.T.);
#16833=ADVANCED_FACE('',(#3024),#365,.T.);
#16834=ADVANCED_FACE('',(#3025),#366,.T.);
#16835=ADVANCED_FACE('',(#3026),#367,.T.);
#16836=ADVANCED_FACE('',(#3027),#368,.T.);
#16837=ADVANCED_FACE('',(#3028),#369,.T.);
#16838=ADVANCED_FACE('',(#3029),#370,.T.);
#16839=ADVANCED_FACE('',(#3030),#371,.T.);
#16840=ADVANCED_FACE('',(#3031),#372,.T.);
#16841=ADVANCED_FACE('',(#3032),#373,.T.);
#16842=ADVANCED_FACE('',(#3033),#15949,.F.);
#16843=ADVANCED_FACE('',(#3034),#78,.F.);
#16844=ADVANCED_FACE('',(#3035),#374,.T.);
#16845=ADVANCED_FACE('',(#3036),#79,.F.);
#16846=ADVANCED_FACE('',(#3037),#375,.T.);
#16847=ADVANCED_FACE('',(#3038),#15950,.T.);
#16848=ADVANCED_FACE('',(#3039),#1029,.T.);
#16849=ADVANCED_FACE('',(#3040),#376,.T.);
#16850=ADVANCED_FACE('',(#3041,#1465),#15951,.T.);
#16851=ADVANCED_FACE('',(#3042),#1030,.T.);
#16852=ADVANCED_FACE('',(#3043),#15952,.T.);
#16853=ADVANCED_FACE('',(#3044),#1031,.T.);
#16854=ADVANCED_FACE('',(#3045),#1032,.T.);
#16855=ADVANCED_FACE('',(#3046),#1033,.T.);
#16856=ADVANCED_FACE('',(#3047,#1466),#15953,.F.);
#16857=ADVANCED_FACE('',(#3048),#377,.F.);
#16858=ADVANCED_FACE('',(#3049),#378,.T.);
#16859=ADVANCED_FACE('',(#3050),#15954,.T.);
#16860=ADVANCED_FACE('',(#3051),#379,.F.);
#16861=ADVANCED_FACE('',(#3052,#1467),#15955,.T.);
#16862=ADVANCED_FACE('',(#3053),#380,.T.);
#16863=ADVANCED_FACE('',(#3054,#1468),#15956,.T.);
#16864=ADVANCED_FACE('',(#3055),#15957,.T.);
#16865=ADVANCED_FACE('',(#3056),#381,.F.);
#16866=ADVANCED_FACE('',(#3057,#1469),#15958,.T.);
#16867=ADVANCED_FACE('',(#3058),#382,.T.);
#16868=ADVANCED_FACE('',(#3059,#1470),#15959,.T.);
#16869=ADVANCED_FACE('',(#3060),#1034,.T.);
#16870=ADVANCED_FACE('',(#3061),#383,.T.);
#16871=ADVANCED_FACE('',(#3062,#1471),#15960,.T.);
#16872=ADVANCED_FACE('',(#3063),#384,.F.);
#16873=ADVANCED_FACE('',(#3064,#1472),#15961,.T.);
#16874=ADVANCED_FACE('',(#3065),#1035,.T.);
#16875=ADVANCED_FACE('',(#3066),#1036,.F.);
#16876=ADVANCED_FACE('',(#3067),#385,.F.);
#16877=ADVANCED_FACE('',(#3068,#1473),#15962,.F.);
#16878=ADVANCED_FACE('',(#3069),#1037,.F.);
#16879=ADVANCED_FACE('',(#3070,#1474),#15963,.T.);
#16880=ADVANCED_FACE('',(#3071),#1038,.T.);
#16881=ADVANCED_FACE('',(#3072),#80,.T.);
#16882=ADVANCED_FACE('',(#3073),#81,.T.);
#16883=ADVANCED_FACE('',(#3074),#1039,.T.);
#16884=ADVANCED_FACE('',(#3075),#1040,.T.);
#16885=ADVANCED_FACE('',(#3076),#1041,.T.);
#16886=ADVANCED_FACE('',(#3077),#1042,.T.);
#16887=ADVANCED_FACE('',(#3078),#1043,.T.);
#16888=ADVANCED_FACE('',(#3079),#1044,.T.);
#16889=ADVANCED_FACE('',(#3080),#82,.T.);
#16890=ADVANCED_FACE('',(#3081),#15964,.T.);
#16891=ADVANCED_FACE('',(#3082),#15965,.T.);
#16892=ADVANCED_FACE('',(#3083),#15966,.T.);
#16893=ADVANCED_FACE('',(#3084),#15967,.T.);
#16894=ADVANCED_FACE('',(#3085),#15968,.T.);
#16895=ADVANCED_FACE('',(#3086),#15969,.T.);
#16896=ADVANCED_FACE('',(#3087),#83,.T.);
#16897=ADVANCED_FACE('',(#3088),#15970,.T.);
#16898=ADVANCED_FACE('',(#3089),#84,.T.);
#16899=ADVANCED_FACE('',(#3090),#15971,.T.);
#16900=ADVANCED_FACE('',(#3091),#15972,.T.);
#16901=ADVANCED_FACE('',(#3092),#85,.T.);
#16902=ADVANCED_FACE('',(#3093),#15973,.T.);
#16903=ADVANCED_FACE('',(#3094),#15974,.T.);
#16904=ADVANCED_FACE('',(#3095),#15975,.T.);
#16905=ADVANCED_FACE('',(#3096),#15976,.T.);
#16906=ADVANCED_FACE('',(#3097),#15977,.T.);
#16907=ADVANCED_FACE('',(#3098),#15978,.T.);
#16908=ADVANCED_FACE('',(#3099),#1045,.T.);
#16909=ADVANCED_FACE('',(#3100),#15979,.T.);
#16910=ADVANCED_FACE('',(#3101),#15980,.T.);
#16911=ADVANCED_FACE('',(#3102),#15981,.T.);
#16912=ADVANCED_FACE('',(#3103),#75,.T.);
#16913=ADVANCED_FACE('',(#3104),#86,.T.);
#16914=ADVANCED_FACE('',(#3105),#15982,.T.);
#16915=ADVANCED_FACE('',(#3106),#15983,.F.);
#16916=ADVANCED_FACE('',(#3107),#386,.T.);
#16917=ADVANCED_FACE('',(#3108),#387,.T.);
#16918=ADVANCED_FACE('',(#3109),#388,.T.);
#16919=ADVANCED_FACE('',(#3110),#389,.T.);
#16920=ADVANCED_FACE('',(#3111),#390,.T.);
#16921=ADVANCED_FACE('',(#3112),#391,.T.);
#16922=ADVANCED_FACE('',(#3113),#392,.T.);
#16923=ADVANCED_FACE('',(#3114),#393,.T.);
#16924=ADVANCED_FACE('',(#3115),#15984,.F.);
#16925=ADVANCED_FACE('',(#3116),#87,.F.);
#16926=ADVANCED_FACE('',(#3117),#15985,.T.);
#16927=ADVANCED_FACE('',(#3118),#394,.T.);
#16928=ADVANCED_FACE('',(#3119),#88,.F.);
#16929=ADVANCED_FACE('',(#3120),#15986,.F.);
#16930=ADVANCED_FACE('',(#3121),#15987,.F.);
#16931=ADVANCED_FACE('',(#3122),#15988,.F.);
#16932=ADVANCED_FACE('',(#3123),#15989,.F.);
#16933=ADVANCED_FACE('',(#3124),#15990,.F.);
#16934=ADVANCED_FACE('',(#3125),#15991,.F.);
#16935=ADVANCED_FACE('',(#3126),#15992,.F.);
#16936=ADVANCED_FACE('',(#3127),#15993,.T.);
#16937=ADVANCED_FACE('',(#3128),#1046,.T.);
#16938=ADVANCED_FACE('',(#3129),#395,.T.);
#16939=ADVANCED_FACE('',(#3130),#1047,.T.);
#16940=ADVANCED_FACE('',(#3131,#1475),#15994,.T.);
#16941=ADVANCED_FACE('',(#3132),#396,.T.);
#16942=ADVANCED_FACE('',(#3133),#397,.T.);
#16943=ADVANCED_FACE('',(#3134),#398,.T.);
#16944=ADVANCED_FACE('',(#3135),#399,.T.);
#16945=ADVANCED_FACE('',(#3136),#400,.T.);
#16946=ADVANCED_FACE('',(#3137),#401,.T.);
#16947=ADVANCED_FACE('',(#3138),#402,.T.);
#16948=ADVANCED_FACE('',(#3139),#403,.T.);
#16949=ADVANCED_FACE('',(#3140),#404,.T.);
#16950=ADVANCED_FACE('',(#3141),#405,.T.);
#16951=ADVANCED_FACE('',(#3142),#406,.T.);
#16952=ADVANCED_FACE('',(#3143),#407,.T.);
#16953=ADVANCED_FACE('',(#3144),#408,.T.);
#16954=ADVANCED_FACE('',(#3145),#409,.T.);
#16955=ADVANCED_FACE('',(#3146),#410,.T.);
#16956=ADVANCED_FACE('',(#3147),#411,.T.);
#16957=ADVANCED_FACE('',(#3148),#412,.T.);
#16958=ADVANCED_FACE('',(#3149),#413,.T.);
#16959=ADVANCED_FACE('',(#3150),#414,.T.);
#16960=ADVANCED_FACE('',(#3151),#415,.T.);
#16961=ADVANCED_FACE('',(#3152),#416,.T.);
#16962=ADVANCED_FACE('',(#3153),#417,.T.);
#16963=ADVANCED_FACE('',(#3154),#418,.T.);
#16964=ADVANCED_FACE('',(#3155),#419,.T.);
#16965=ADVANCED_FACE('',(#3156),#420,.T.);
#16966=ADVANCED_FACE('',(#3157),#421,.T.);
#16967=ADVANCED_FACE('',(#3158),#422,.T.);
#16968=ADVANCED_FACE('',(#3159),#423,.T.);
#16969=ADVANCED_FACE('',(#3160),#424,.T.);
#16970=ADVANCED_FACE('',(#3161),#89,.F.);
#16971=ADVANCED_FACE('',(#3162),#15995,.T.);
#16972=ADVANCED_FACE('',(#3163),#425,.T.);
#16973=ADVANCED_FACE('',(#3164),#90,.F.);
#16974=ADVANCED_FACE('',(#3165),#15996,.F.);
#16975=ADVANCED_FACE('',(#3166),#15997,.T.);
#16976=ADVANCED_FACE('',(#3167),#15998,.F.);
#16977=ADVANCED_FACE('',(#3168),#426,.T.);
#16978=ADVANCED_FACE('',(#3169),#15999,.F.);
#16979=ADVANCED_FACE('',(#3170),#16000,.T.);
#16980=ADVANCED_FACE('',(#3171),#16001,.F.);
#16981=ADVANCED_FACE('',(#3172),#16002,.F.);
#16982=ADVANCED_FACE('',(#3173),#16003,.T.);
#16983=ADVANCED_FACE('',(#3174),#16004,.F.);
#16984=ADVANCED_FACE('',(#3175),#16005,.F.);
#16985=ADVANCED_FACE('',(#3176),#16006,.T.);
#16986=ADVANCED_FACE('',(#3177),#16007,.F.);
#16987=ADVANCED_FACE('',(#3178),#16008,.F.);
#16988=ADVANCED_FACE('',(#3179),#16009,.T.);
#16989=ADVANCED_FACE('',(#3180),#16010,.F.);
#16990=ADVANCED_FACE('',(#3181),#16011,.F.);
#16991=ADVANCED_FACE('',(#3182),#16012,.T.);
#16992=ADVANCED_FACE('',(#3183),#16013,.F.);
#16993=ADVANCED_FACE('',(#3184),#16014,.F.);
#16994=ADVANCED_FACE('',(#3185),#16015,.T.);
#16995=ADVANCED_FACE('',(#3186),#16016,.F.);
#16996=ADVANCED_FACE('',(#3187),#16017,.F.);
#16997=ADVANCED_FACE('',(#3188),#16018,.T.);
#16998=ADVANCED_FACE('',(#3189),#16019,.F.);
#16999=ADVANCED_FACE('',(#3190),#16020,.F.);
#17000=ADVANCED_FACE('',(#3191),#16021,.T.);
#17001=ADVANCED_FACE('',(#3192),#16022,.F.);
#17002=ADVANCED_FACE('',(#3193),#16023,.F.);
#17003=ADVANCED_FACE('',(#3194),#16024,.T.);
#17004=ADVANCED_FACE('',(#3195),#16025,.F.);
#17005=ADVANCED_FACE('',(#3196),#16026,.F.);
#17006=ADVANCED_FACE('',(#3197),#16027,.T.);
#17007=ADVANCED_FACE('',(#3198),#16028,.F.);
#17008=ADVANCED_FACE('',(#3199),#16029,.F.);
#17009=ADVANCED_FACE('',(#3200),#16030,.T.);
#17010=ADVANCED_FACE('',(#3201),#16031,.F.);
#17011=ADVANCED_FACE('',(#3202),#16032,.F.);
#17012=ADVANCED_FACE('',(#3203),#16033,.T.);
#17013=ADVANCED_FACE('',(#3204),#16034,.F.);
#17014=ADVANCED_FACE('',(#3205),#16035,.F.);
#17015=ADVANCED_FACE('',(#3206),#16036,.T.);
#17016=ADVANCED_FACE('',(#3207),#16037,.F.);
#17017=ADVANCED_FACE('',(#3208),#16038,.F.);
#17018=ADVANCED_FACE('',(#3209),#16039,.T.);
#17019=ADVANCED_FACE('',(#3210),#16040,.F.);
#17020=ADVANCED_FACE('',(#3211),#16041,.F.);
#17021=ADVANCED_FACE('',(#3212),#16042,.T.);
#17022=ADVANCED_FACE('',(#3213),#16043,.F.);
#17023=ADVANCED_FACE('',(#3214),#16044,.F.);
#17024=ADVANCED_FACE('',(#3215),#16045,.T.);
#17025=ADVANCED_FACE('',(#3216),#16046,.F.);
#17026=ADVANCED_FACE('',(#3217),#16047,.F.);
#17027=ADVANCED_FACE('',(#3218),#16048,.T.);
#17028=ADVANCED_FACE('',(#3219),#16049,.F.);
#17029=ADVANCED_FACE('',(#3220),#16050,.F.);
#17030=ADVANCED_FACE('',(#3221),#16051,.T.);
#17031=ADVANCED_FACE('',(#3222),#16052,.F.);
#17032=ADVANCED_FACE('',(#3223),#16053,.F.);
#17033=ADVANCED_FACE('',(#3224),#16054,.T.);
#17034=ADVANCED_FACE('',(#3225),#16055,.F.);
#17035=ADVANCED_FACE('',(#3226),#16056,.F.);
#17036=ADVANCED_FACE('',(#3227),#16057,.T.);
#17037=ADVANCED_FACE('',(#3228),#16058,.F.);
#17038=ADVANCED_FACE('',(#3229),#16059,.F.);
#17039=ADVANCED_FACE('',(#3230),#16060,.T.);
#17040=ADVANCED_FACE('',(#3231),#16061,.F.);
#17041=ADVANCED_FACE('',(#3232),#16062,.F.);
#17042=ADVANCED_FACE('',(#3233),#16063,.T.);
#17043=ADVANCED_FACE('',(#3234),#16064,.F.);
#17044=ADVANCED_FACE('',(#3235),#16065,.F.);
#17045=ADVANCED_FACE('',(#3236),#16066,.T.);
#17046=ADVANCED_FACE('',(#3237),#16067,.F.);
#17047=ADVANCED_FACE('',(#3238),#16068,.F.);
#17048=ADVANCED_FACE('',(#3239),#16069,.T.);
#17049=ADVANCED_FACE('',(#3240),#16070,.F.);
#17050=ADVANCED_FACE('',(#3241),#16071,.F.);
#17051=ADVANCED_FACE('',(#3242),#16072,.T.);
#17052=ADVANCED_FACE('',(#3243),#16073,.F.);
#17053=ADVANCED_FACE('',(#3244),#16074,.F.);
#17054=ADVANCED_FACE('',(#3245),#16075,.T.);
#17055=ADVANCED_FACE('',(#3246),#16076,.F.);
#17056=ADVANCED_FACE('',(#3247),#16077,.F.);
#17057=ADVANCED_FACE('',(#3248),#16078,.T.);
#17058=ADVANCED_FACE('',(#3249),#16079,.F.);
#17059=ADVANCED_FACE('',(#3250),#16080,.F.);
#17060=ADVANCED_FACE('',(#3251),#16081,.T.);
#17061=ADVANCED_FACE('',(#3252),#16082,.F.);
#17062=ADVANCED_FACE('',(#3253),#16083,.F.);
#17063=ADVANCED_FACE('',(#3254),#16084,.T.);
#17064=ADVANCED_FACE('',(#3255),#16085,.F.);
#17065=ADVANCED_FACE('',(#3256),#16086,.T.);
#17066=ADVANCED_FACE('',(#3257),#1048,.T.);
#17067=ADVANCED_FACE('',(#3258),#427,.T.);
#17068=ADVANCED_FACE('',(#3259,#1476),#16087,.T.);
#17069=ADVANCED_FACE('',(#3260),#1049,.T.);
#17070=ADVANCED_FACE('',(#3261),#1050,.T.);
#17071=ADVANCED_FACE('',(#3262),#16088,.T.);
#17072=CLOSED_SHELL('',(#16089,#16090,#16091,#16092,#16093,#16094,#16095,
#16096,#16097,#16098,#16099,#16100,#16101,#16102,#16103,#16104,#16105,#16106,
#16107,#16108,#16109,#16110,#16111,#16112,#16113,#16114,#16115,#16116,#16117,
#16118,#16119,#16120,#16121,#16122,#16123,#16124,#16125,#16126,#16127,#16128,
#16129,#16130,#16131,#16132,#16133,#16134,#16135,#16136,#16137,#16138,#16139,
#16140,#16141,#16142,#16143,#16144,#16145,#16146,#16147,#16148,#16149,#16150,
#16151,#16152,#16153,#16154,#16155,#16156,#16157,#16158,#16159,#16160));
#17073=CLOSED_SHELL('',(#16161,#16162,#16163,#16164,#16165,#16166,#16167,
#16168,#16169,#16170,#16171,#16172,#16173,#16174,#16175,#16176,#16177,#16178,
#16179,#16180,#16181,#16182,#16183,#16184,#16185,#16186,#16187,#16188,#16189,
#16190,#16191,#16192,#16193,#16194,#16195,#16196,#16197,#16198,#16199,#16200,
#16201,#16202,#16203,#16204,#16205,#16206,#16207,#16208,#16209,#16210,#16211,
#16212,#16213,#16214,#16215,#16216,#16217,#16218,#16219,#16220,#16221,#16222,
#16223,#16224,#16225,#16226,#16227,#16228,#16229,#16230,#16231,#16232,#16233,
#16234,#16235,#16236,#16237,#16238,#16239,#16240,#16241,#16242,#16243,#16244,
#16245,#16246,#16247,#16248,#16249,#16250,#16251,#16252,#16253,#16254,#16255,
#16256,#16257,#16258,#16259,#16260,#16261,#16262,#16263,#16264,#16265,#16266,
#16267,#16268,#16269,#16270,#16271,#16272,#16273,#16274,#16275,#16276,#16277,
#16278,#16279,#16280,#16281,#16282,#16283,#16284,#16285,#16286,#16287,#16288,
#16289,#16290,#16291,#16292,#16293,#16294,#16295,#16296,#16297,#16298,#16299,
#16300,#16301,#16302,#16303,#16304,#16305,#16306,#16307,#16308,#16309,#16310,
#16311,#16312,#16313,#16314,#16315,#16316,#16317,#16318,#16319,#16320,#16321,
#16322,#16323,#16324,#16325,#16326,#16327,#16328,#16329,#16330,#16331,#16332,
#16333,#16334,#16335,#16336,#16337,#16338,#16339,#16340,#16341,#16342,#16343,
#16344,#16345,#16346,#16347,#16348,#16349,#16350,#16351,#16352,#16353,#16354,
#16355,#16356,#16357,#16358,#16359,#16360,#16361,#16362,#16363,#16364,#16365,
#16366,#16367,#16368,#16369,#16370,#16371,#16372,#16373,#16374,#16375,#16376,
#16377,#16378,#16379,#16380,#16381,#16382,#16383,#16384,#16385,#16386,#16387,
#16388,#16389,#16390,#16391,#16392,#16393,#16394,#16395,#16396,#16397,#16398,
#16399,#16400,#16401,#16402,#16403,#16404,#16405,#16406,#16407,#16408,#16409,
#16410,#16411,#16412,#16413,#16414,#16415,#16416,#16417,#16418,#16419,#16420,
#16421,#16422,#16423,#16424,#16425,#16426,#16427,#16428,#16429,#16430,#16431,
#16432,#16433,#16434,#16435,#16436,#16437,#16438,#16439,#16440,#16441,#16442,
#16443,#16444,#16445,#16446,#16447,#16448,#16449,#16450,#16451,#16452,#16453,
#16454,#16455,#16456,#16457,#16458,#16459,#16460,#16461,#16462,#16463,#16464,
#16465,#16466,#16467,#16468,#16469,#16470,#16471,#16472,#16473,#16474,#16475,
#16476,#16477,#16478,#16479,#16480,#16481,#16482,#16483,#16484,#16485,#16486,
#16487,#16488,#16489,#16490,#16491,#16492,#16493,#16494,#16495,#16496,#16497,
#16498,#16499,#16500,#16501,#16502,#16503,#16504,#16505,#16506,#16507,#16508,
#16509,#16510,#16511,#16512,#16513,#16514,#16515,#16516,#16517,#16518,#16519,
#16520,#16521,#16522,#16523,#16524,#16525,#16526,#16527,#16528,#16529,#16530,
#16531,#16532,#16533,#16534,#16535,#16536,#16537,#16538,#16539,#16540,#16541,
#16542,#16543,#16544,#16545,#16546,#16547,#16548,#16549,#16550,#16551,#16552,
#16553,#16554,#16555,#16556,#16557,#16558,#16559,#16560,#16561,#16562,#16563,
#16564,#16565,#16566,#16567,#16568,#16569,#16570,#16571,#16572,#16573,#16574,
#16575,#16576,#16577,#16578,#16579,#16580,#16581,#16582,#16583,#16584,#16585,
#16586,#16587,#16588,#16589,#16590,#16591,#16592,#16593,#16594,#16595,#16596,
#16597,#16598,#16599,#16600,#16601,#16602,#16603,#16604,#16605,#16606,#16607,
#16608,#16609,#16610,#16611,#16612,#16613,#16614,#16615,#16616,#16617,#16618,
#16619,#16620,#16621,#16622,#16623,#16624,#16625,#16626,#16627,#16628,#16629,
#16630,#16631,#16632,#16633,#16634,#16635,#16636,#16637,#16638,#16639,#16640,
#16641,#16642,#16643,#16644,#16645,#16646,#16647,#16648,#16649,#16650,#16651,
#16652,#16653,#16654,#16655,#16656,#16657,#16658,#16659,#16660,#16661,#16662,
#16663,#16664,#16665,#16666,#16667,#16668,#16669,#16670,#16671,#16672,#16673,
#16674,#16675,#16676,#16677,#16678,#16679,#16680,#16681,#16682,#16683,#16684,
#16685,#16686,#16687,#16688,#16689,#16690,#16691,#16692,#16693,#16694,#16695,
#16696,#16697,#16698,#16699,#16700,#16701,#16702,#16703,#16704,#16705,#16706,
#16707,#16708,#16709,#16710,#16711,#16712,#16713,#16714,#16715,#16716,#16717,
#16718,#16719,#16720,#16721,#16722,#16723,#16724,#16725,#16726,#16727,#16728,
#16729,#16730,#16731,#16732,#16733,#16734,#16735,#16736,#16737,#16738,#16739,
#16740,#16741,#16742,#16743,#16744,#16745,#16746,#16747,#16748,#16749,#16750,
#16751,#16752,#16753,#16754,#16755,#16756,#16757,#16758,#16759,#16760,#16761,
#16762,#16763,#16764,#16765,#16766,#16767,#16768,#16769,#16770,#16771,#16772,
#16773,#16774,#16775,#16776,#16777,#16778,#16779,#16780,#16781,#16782,#16783,
#16784,#16785,#16786,#16787,#16788,#16789,#16790,#16791,#16792,#16793,#16794,
#16795));
#17074=CLOSED_SHELL('',(#16796,#16797,#16798,#16799,#16800,#16801,#16802,
#16803,#16804,#16805,#16806,#16807,#16808,#16809,#16810,#16811,#16812,#16813,
#16814,#16815,#16816,#16817,#16818,#16819,#16820,#16821,#16822,#16823,#16824,
#16825,#16826,#16827,#16828,#16829));
#17075=CLOSED_SHELL('',(#16830,#16831,#16832,#16833,#16834,#16835,#16836,
#16837,#16838,#16839,#16840,#16841,#16842,#16843,#16844,#16845,#16846,#16847,
#16848,#16849,#16850,#16851,#16852));
#17076=CLOSED_SHELL('',(#16853,#16854,#16855,#16856,#16857,#16858,#16859,
#16860,#16861,#16862,#16863,#16864));
#17077=CLOSED_SHELL('',(#16865,#16866,#16867,#16868));
#17078=CLOSED_SHELL('',(#16869,#16870,#16871,#16872,#16873,#16874));
#17079=CLOSED_SHELL('',(#16875,#16876,#16877,#16878,#16879,#16880,#16881,
#16882,#16883,#16884,#16885,#16886,#16887,#16888,#16889,#16890,#16891,#16892,
#16893,#16894,#16895,#16896,#16897,#16898,#16899,#16900,#16901,#16902,#16903,
#16904,#16905,#16906,#16907,#16908,#16909,#16910,#16911));
#17080=CLOSED_SHELL('',(#16912));
#17081=CLOSED_SHELL('',(#16913,#16914,#16915));
#17082=CLOSED_SHELL('',(#16916,#16917,#16918,#16919,#16920,#16921,#16922,
#16923,#16924,#16925,#16926,#16927,#16928,#16929,#16930,#16931,#16932,#16933,
#16934,#16935,#16936,#16937,#16938,#16939,#16940));
#17083=CLOSED_SHELL('',(#16941,#16942,#16943,#16944,#16945,#16946,#16947,
#16948,#16949,#16950,#16951,#16952,#16953,#16954,#16955,#16956,#16957,#16958,
#16959,#16960,#16961,#16962,#16963,#16964,#16965,#16966,#16967,#16968,#16969,
#16970,#16971,#16972,#16973,#16974,#16975,#16976,#16977,#16978,#16979,#16980,
#16981,#16982,#16983,#16984,#16985,#16986,#16987,#16988,#16989,#16990,#16991,
#16992,#16993,#16994,#16995,#16996,#16997,#16998,#16999,#17000,#17001,#17002,
#17003,#17004,#17005,#17006,#17007,#17008,#17009,#17010,#17011,#17012,#17013,
#17014,#17015,#17016,#17017,#17018,#17019,#17020,#17021,#17022,#17023,#17024,
#17025,#17026,#17027,#17028,#17029,#17030,#17031,#17032,#17033,#17034,#17035,
#17036,#17037,#17038,#17039,#17040,#17041,#17042,#17043,#17044,#17045,#17046,
#17047,#17048,#17049,#17050,#17051,#17052,#17053,#17054,#17055,#17056,#17057,
#17058,#17059,#17060,#17061,#17062,#17063,#17064,#17065,#17066,#17067,#17068,
#17069,#17070,#17071));
#17084=DERIVED_UNIT_ELEMENT(#17108,1.);
#17085=DERIVED_UNIT_ELEMENT(#38530,-3.);
#17086=DERIVED_UNIT_ELEMENT(#17108,1.);
#17087=DERIVED_UNIT_ELEMENT(#38530,-3.);
#17088=DERIVED_UNIT_ELEMENT(#17108,1.);
#17089=DERIVED_UNIT_ELEMENT(#38530,-3.);
#17090=DERIVED_UNIT_ELEMENT(#17108,1.);
#17091=DERIVED_UNIT_ELEMENT(#38530,-3.);
#17092=DERIVED_UNIT_ELEMENT(#17108,1.);
#17093=DERIVED_UNIT_ELEMENT(#38530,-3.);
#17094=DERIVED_UNIT_ELEMENT(#17108,1.);
#17095=DERIVED_UNIT_ELEMENT(#38530,-3.);
#17096=DERIVED_UNIT_ELEMENT(#17108,1.);
#17097=DERIVED_UNIT_ELEMENT(#38530,-3.);
#17098=DERIVED_UNIT_ELEMENT(#17108,1.);
#17099=DERIVED_UNIT_ELEMENT(#38530,-3.);
#17100=DERIVED_UNIT_ELEMENT(#17108,1.);
#17101=DERIVED_UNIT_ELEMENT(#38530,-3.);
#17102=DERIVED_UNIT_ELEMENT(#17108,1.);
#17103=DERIVED_UNIT_ELEMENT(#38530,-3.);
#17104=DERIVED_UNIT_ELEMENT(#17108,1.);
#17105=DERIVED_UNIT_ELEMENT(#38530,-3.);
#17106=DERIVED_UNIT_ELEMENT(#17108,1.);
#17107=DERIVED_UNIT_ELEMENT(#38530,-3.);
#17108=(
MASS_UNIT()
NAMED_UNIT(*)
SI_UNIT(.KILO.,.GRAM.)
);
#17109=DERIVED_UNIT((#17084,#17085));
#17110=DERIVED_UNIT((#17086,#17087));
#17111=DERIVED_UNIT((#17088,#17089));
#17112=DERIVED_UNIT((#17090,#17091));
#17113=DERIVED_UNIT((#17092,#17093));
#17114=DERIVED_UNIT((#17094,#17095));
#17115=DERIVED_UNIT((#17096,#17097));
#17116=DERIVED_UNIT((#17098,#17099));
#17117=DERIVED_UNIT((#17100,#17101));
#17118=DERIVED_UNIT((#17102,#17103));
#17119=DERIVED_UNIT((#17104,#17105));
#17120=DERIVED_UNIT((#17106,#17107));
#17121=MEASURE_REPRESENTATION_ITEM('density measure',
POSITIVE_RATIO_MEASURE(7850.),#17109);
#17122=MEASURE_REPRESENTATION_ITEM('density measure',
POSITIVE_RATIO_MEASURE(7850.),#17110);
#17123=MEASURE_REPRESENTATION_ITEM('density measure',
POSITIVE_RATIO_MEASURE(7850.),#17111);
#17124=MEASURE_REPRESENTATION_ITEM('density measure',
POSITIVE_RATIO_MEASURE(7850.),#17112);
#17125=MEASURE_REPRESENTATION_ITEM('density measure',
POSITIVE_RATIO_MEASURE(7850.),#17113);
#17126=MEASURE_REPRESENTATION_ITEM('density measure',
POSITIVE_RATIO_MEASURE(7850.),#17114);
#17127=MEASURE_REPRESENTATION_ITEM('density measure',
POSITIVE_RATIO_MEASURE(7850.),#17115);
#17128=MEASURE_REPRESENTATION_ITEM('density measure',
POSITIVE_RATIO_MEASURE(7850.),#17116);
#17129=MEASURE_REPRESENTATION_ITEM('density measure',
POSITIVE_RATIO_MEASURE(7850.),#17117);
#17130=MEASURE_REPRESENTATION_ITEM('density measure',
POSITIVE_RATIO_MEASURE(7850.),#17118);
#17131=MEASURE_REPRESENTATION_ITEM('density measure',
POSITIVE_RATIO_MEASURE(7850.),#17119);
#17132=MEASURE_REPRESENTATION_ITEM('density measure',
POSITIVE_RATIO_MEASURE(7850.),#17120);
#17133=PROPERTY_DEFINITION_REPRESENTATION(#17193,#17157);
#17134=PROPERTY_DEFINITION_REPRESENTATION(#17194,#17158);
#17135=PROPERTY_DEFINITION_REPRESENTATION(#17195,#17159);
#17136=PROPERTY_DEFINITION_REPRESENTATION(#17196,#17160);
#17137=PROPERTY_DEFINITION_REPRESENTATION(#17197,#17161);
#17138=PROPERTY_DEFINITION_REPRESENTATION(#17198,#17162);
#17139=PROPERTY_DEFINITION_REPRESENTATION(#17199,#17163);
#17140=PROPERTY_DEFINITION_REPRESENTATION(#17200,#17164);
#17141=PROPERTY_DEFINITION_REPRESENTATION(#17201,#17165);
#17142=PROPERTY_DEFINITION_REPRESENTATION(#17202,#17166);
#17143=PROPERTY_DEFINITION_REPRESENTATION(#17203,#17167);
#17144=PROPERTY_DEFINITION_REPRESENTATION(#17204,#17168);
#17145=PROPERTY_DEFINITION_REPRESENTATION(#17205,#17169);
#17146=PROPERTY_DEFINITION_REPRESENTATION(#17206,#17170);
#17147=PROPERTY_DEFINITION_REPRESENTATION(#17207,#17171);
#17148=PROPERTY_DEFINITION_REPRESENTATION(#17208,#17172);
#17149=PROPERTY_DEFINITION_REPRESENTATION(#17209,#17173);
#17150=PROPERTY_DEFINITION_REPRESENTATION(#17210,#17174);
#17151=PROPERTY_DEFINITION_REPRESENTATION(#17211,#17175);
#17152=PROPERTY_DEFINITION_REPRESENTATION(#17212,#17176);
#17153=PROPERTY_DEFINITION_REPRESENTATION(#17213,#17177);
#17154=PROPERTY_DEFINITION_REPRESENTATION(#17214,#17178);
#17155=PROPERTY_DEFINITION_REPRESENTATION(#17215,#17179);
#17156=PROPERTY_DEFINITION_REPRESENTATION(#17216,#17180);
#17157=REPRESENTATION('material name',(#17181),#38516);
#17158=REPRESENTATION('density',(#17121),#38516);
#17159=REPRESENTATION('material name',(#17182),#38517);
#17160=REPRESENTATION('density',(#17122),#38517);
#17161=REPRESENTATION('material name',(#17183),#38518);
#17162=REPRESENTATION('density',(#17123),#38518);
#17163=REPRESENTATION('material name',(#17184),#38519);
#17164=REPRESENTATION('density',(#17124),#38519);
#17165=REPRESENTATION('material name',(#17185),#38520);
#17166=REPRESENTATION('density',(#17125),#38520);
#17167=REPRESENTATION('material name',(#17186),#38521);
#17168=REPRESENTATION('density',(#17126),#38521);
#17169=REPRESENTATION('material name',(#17187),#38522);
#17170=REPRESENTATION('density',(#17127),#38522);
#17171=REPRESENTATION('material name',(#17188),#38523);
#17172=REPRESENTATION('density',(#17128),#38523);
#17173=REPRESENTATION('material name',(#17189),#38524);
#17174=REPRESENTATION('density',(#17129),#38524);
#17175=REPRESENTATION('material name',(#17190),#38525);
#17176=REPRESENTATION('density',(#17130),#38525);
#17177=REPRESENTATION('material name',(#17191),#38526);
#17178=REPRESENTATION('density',(#17131),#38526);
#17179=REPRESENTATION('material name',(#17192),#38527);
#17180=REPRESENTATION('density',(#17132),#38527);
#17181=DESCRIPTIVE_REPRESENTATION_ITEM('Steel','Steel');
#17182=DESCRIPTIVE_REPRESENTATION_ITEM('Steel','Steel');
#17183=DESCRIPTIVE_REPRESENTATION_ITEM('Steel','Steel');
#17184=DESCRIPTIVE_REPRESENTATION_ITEM('Steel','Steel');
#17185=DESCRIPTIVE_REPRESENTATION_ITEM('Steel','Steel');
#17186=DESCRIPTIVE_REPRESENTATION_ITEM('Steel','Steel');
#17187=DESCRIPTIVE_REPRESENTATION_ITEM('Steel','Steel');
#17188=DESCRIPTIVE_REPRESENTATION_ITEM('Steel','Steel');
#17189=DESCRIPTIVE_REPRESENTATION_ITEM('Steel','Steel');
#17190=DESCRIPTIVE_REPRESENTATION_ITEM('Steel','Steel');
#17191=DESCRIPTIVE_REPRESENTATION_ITEM('Steel','Steel');
#17192=DESCRIPTIVE_REPRESENTATION_ITEM('Steel','Steel');
#17193=PROPERTY_DEFINITION('material property','material name',#38590);
#17194=PROPERTY_DEFINITION('material property','density of part',#38590);
#17195=PROPERTY_DEFINITION('material property','material name',#38591);
#17196=PROPERTY_DEFINITION('material property','density of part',#38591);
#17197=PROPERTY_DEFINITION('material property','material name',#38592);
#17198=PROPERTY_DEFINITION('material property','density of part',#38592);
#17199=PROPERTY_DEFINITION('material property','material name',#38593);
#17200=PROPERTY_DEFINITION('material property','density of part',#38593);
#17201=PROPERTY_DEFINITION('material property','material name',#38594);
#17202=PROPERTY_DEFINITION('material property','density of part',#38594);
#17203=PROPERTY_DEFINITION('material property','material name',#38595);
#17204=PROPERTY_DEFINITION('material property','density of part',#38595);
#17205=PROPERTY_DEFINITION('material property','material name',#38596);
#17206=PROPERTY_DEFINITION('material property','density of part',#38596);
#17207=PROPERTY_DEFINITION('material property','material name',#38597);
#17208=PROPERTY_DEFINITION('material property','density of part',#38597);
#17209=PROPERTY_DEFINITION('material property','material name',#38598);
#17210=PROPERTY_DEFINITION('material property','density of part',#38598);
#17211=PROPERTY_DEFINITION('material property','material name',#38599);
#17212=PROPERTY_DEFINITION('material property','density of part',#38599);
#17213=PROPERTY_DEFINITION('material property','material name',#38600);
#17214=PROPERTY_DEFINITION('material property','density of part',#38600);
#17215=PROPERTY_DEFINITION('material property','material name',#38601);
#17216=PROPERTY_DEFINITION('material property','density of part',#38601);
#17217=AXIS2_PLACEMENT_3D('',#23616,#19025,#19026);
#17218=AXIS2_PLACEMENT_3D('',#23617,#19027,#19028);
#17219=AXIS2_PLACEMENT_3D('',#23618,#19029,#19030);
#17220=AXIS2_PLACEMENT_3D('',#23627,#19035,#19036);
#17221=AXIS2_PLACEMENT_3D('',#23636,#19041,#19042);
#17222=AXIS2_PLACEMENT_3D('',#23639,#19045,#19046);
#17223=AXIS2_PLACEMENT_3D('',#23642,#19049,#19050);
#17224=AXIS2_PLACEMENT_3D('',#23648,#19054,#19055);
#17225=AXIS2_PLACEMENT_3D('',#23652,#19058,#19059);
#17226=AXIS2_PLACEMENT_3D('',#23661,#19063,#19064);
#17227=AXIS2_PLACEMENT_3D('',#23662,#19065,#19066);
#17228=AXIS2_PLACEMENT_3D('',#23687,#19079,#19080);
#17229=AXIS2_PLACEMENT_3D('',#23693,#19084,#19085);
#17230=AXIS2_PLACEMENT_3D('',#23697,#19088,#19089);
#17231=AXIS2_PLACEMENT_3D('',#23701,#19092,#19093);
#17232=AXIS2_PLACEMENT_3D('',#23707,#19097,#19098);
#17233=AXIS2_PLACEMENT_3D('',#23711,#19101,#19102);
#17234=AXIS2_PLACEMENT_3D('',#23715,#19105,#19106);
#17235=AXIS2_PLACEMENT_3D('',#23721,#19110,#19111);
#17236=AXIS2_PLACEMENT_3D('',#23727,#19115,#19116);
#17237=AXIS2_PLACEMENT_3D('',#23733,#19120,#19121);
#17238=AXIS2_PLACEMENT_3D('',#23739,#19125,#19126);
#17239=AXIS2_PLACEMENT_3D('',#23745,#19130,#19131);
#17240=AXIS2_PLACEMENT_3D('',#23751,#19135,#19136);
#17241=AXIS2_PLACEMENT_3D('',#23757,#19140,#19141);
#17242=AXIS2_PLACEMENT_3D('',#23763,#19145,#19146);
#17243=AXIS2_PLACEMENT_3D('',#23769,#19150,#19151);
#17244=AXIS2_PLACEMENT_3D('',#23771,#19152,#19153);
#17245=AXIS2_PLACEMENT_3D('',#23773,#19155,#19156);
#17246=AXIS2_PLACEMENT_3D('',#23779,#19160,#19161);
#17247=AXIS2_PLACEMENT_3D('',#23781,#19162,#19163);
#17248=AXIS2_PLACEMENT_3D('',#23783,#19165,#19166);
#17249=AXIS2_PLACEMENT_3D('',#23791,#19171,#19172);
#17250=AXIS2_PLACEMENT_3D('',#23793,#19174,#19175);
#17251=AXIS2_PLACEMENT_3D('',#23801,#19180,#19181);
#17252=AXIS2_PLACEMENT_3D('',#23808,#19183,#19184);
#17253=AXIS2_PLACEMENT_3D('',#23809,#19185,#19186);
#17254=AXIS2_PLACEMENT_3D('',#23814,#19189,#19190);
#17255=AXIS2_PLACEMENT_3D('',#23815,#19191,#19192);
#17256=AXIS2_PLACEMENT_3D('',#23824,#19193,#19194);
#17257=AXIS2_PLACEMENT_3D('',#23825,#19195,#19196);
#17258=AXIS2_PLACEMENT_3D('',#23826,#19197,#19198);
#17259=AXIS2_PLACEMENT_3D('',#23830,#19200,#19201);
#17260=AXIS2_PLACEMENT_3D('',#23832,#19202,#19203);
#17261=AXIS2_PLACEMENT_3D('',#23834,#19204,#19205);
#17262=AXIS2_PLACEMENT_3D('',#23875,#19207,#19208);
#17263=AXIS2_PLACEMENT_3D('',#23880,#19211,#19212);
#17264=AXIS2_PLACEMENT_3D('',#23883,#19214,#19215);
#17265=AXIS2_PLACEMENT_3D('',#23885,#19216,#19217);
#17266=AXIS2_PLACEMENT_3D('',#23886,#19218,#19219);
#17267=AXIS2_PLACEMENT_3D('',#23892,#19220,#19221);
#17268=AXIS2_PLACEMENT_3D('',#23893,#19222,#19223);
#17269=AXIS2_PLACEMENT_3D('',#23894,#19224,#19225);
#17270=AXIS2_PLACEMENT_3D('',#23896,#19227,#19228);
#17271=AXIS2_PLACEMENT_3D('',#23898,#19230,#19231);
#17272=AXIS2_PLACEMENT_3D('',#23900,#19233,#19234);
#17273=AXIS2_PLACEMENT_3D('',#23902,#19236,#19237);
#17274=AXIS2_PLACEMENT_3D('',#23904,#19239,#19240);
#17275=AXIS2_PLACEMENT_3D('',#23906,#19242,#19243);
#17276=AXIS2_PLACEMENT_3D('',#23908,#19245,#19246);
#17277=AXIS2_PLACEMENT_3D('',#23910,#19248,#19249);
#17278=AXIS2_PLACEMENT_3D('',#23912,#19251,#19252);
#17279=AXIS2_PLACEMENT_3D('',#23914,#19254,#19255);
#17280=AXIS2_PLACEMENT_3D('',#23917,#19257,#19258);
#17281=AXIS2_PLACEMENT_3D('',#23918,#19259,#19260);
#17282=AXIS2_PLACEMENT_3D('',#23921,#19262,#19263);
#17283=AXIS2_PLACEMENT_3D('',#23922,#19264,#19265);
#17284=AXIS2_PLACEMENT_3D('',#23925,#19268,#19269);
#17285=AXIS2_PLACEMENT_3D('',#23926,#19270,#19271);
#17286=AXIS2_PLACEMENT_3D('',#23927,#19272,#19273);
#17287=AXIS2_PLACEMENT_3D('',#23929,#19275,#19276);
#17288=AXIS2_PLACEMENT_3D('',#23930,#19277,#19278);
#17289=AXIS2_PLACEMENT_3D('',#23932,#19280,#19281);
#17290=AXIS2_PLACEMENT_3D('',#23934,#19282,#19283);
#17291=AXIS2_PLACEMENT_3D('',#23935,#19284,#19285);
#17292=AXIS2_PLACEMENT_3D('',#23937,#19286,#19287);
#17293=AXIS2_PLACEMENT_3D('',#23940,#19289,#19290);
#17294=AXIS2_PLACEMENT_3D('',#23941,#19291,#19292);
#17295=AXIS2_PLACEMENT_3D('',#23943,#19293,#19294);
#17296=AXIS2_PLACEMENT_3D('',#23945,#19296,#19297);
#17297=AXIS2_PLACEMENT_3D('',#23947,#19299,#19300);
#17298=AXIS2_PLACEMENT_3D('',#23950,#19302,#19303);
#17299=AXIS2_PLACEMENT_3D('',#23951,#19304,#19305);
#17300=AXIS2_PLACEMENT_3D('',#23953,#19306,#19307);
#17301=AXIS2_PLACEMENT_3D('',#23955,#19309,#19310);
#17302=AXIS2_PLACEMENT_3D('',#23958,#19312,#19313);
#17303=AXIS2_PLACEMENT_3D('',#23959,#19314,#19315);
#17304=AXIS2_PLACEMENT_3D('',#23961,#19316,#19317);
#17305=AXIS2_PLACEMENT_3D('',#23963,#19318,#19319);
#17306=AXIS2_PLACEMENT_3D('',#23965,#19320,#19321);
#17307=AXIS2_PLACEMENT_3D('',#23966,#19322,#19323);
#17308=AXIS2_PLACEMENT_3D('',#23968,#19325,#19326);
#17309=AXIS2_PLACEMENT_3D('',#23971,#19328,#19329);
#17310=AXIS2_PLACEMENT_3D('',#23972,#19330,#19331);
#17311=AXIS2_PLACEMENT_3D('',#23973,#19332,#19333);
#17312=AXIS2_PLACEMENT_3D('',#23975,#19334,#19335);
#17313=AXIS2_PLACEMENT_3D('',#23976,#19336,#19337);
#17314=AXIS2_PLACEMENT_3D('',#23978,#19339,#19340);
#17315=AXIS2_PLACEMENT_3D('',#23981,#19342,#19343);
#17316=AXIS2_PLACEMENT_3D('',#23982,#19344,#19345);
#17317=AXIS2_PLACEMENT_3D('',#23983,#19346,#19347);
#17318=AXIS2_PLACEMENT_3D('',#23984,#19348,#19349);
#17319=AXIS2_PLACEMENT_3D('',#23985,#19350,#19351);
#17320=AXIS2_PLACEMENT_3D('',#23986,#19352,#19353);
#17321=AXIS2_PLACEMENT_3D('',#23990,#19356,#19357);
#17322=AXIS2_PLACEMENT_3D('',#23992,#19359,#19360);
#17323=AXIS2_PLACEMENT_3D('',#23993,#19361,#19362);
#17324=AXIS2_PLACEMENT_3D('',#23994,#19363,#19364);
#17325=AXIS2_PLACEMENT_3D('',#24005,#19368,#19369);
#17326=AXIS2_PLACEMENT_3D('',#24007,#19370,#19371);
#17327=AXIS2_PLACEMENT_3D('',#24010,#19373,#19374);
#17328=AXIS2_PLACEMENT_3D('',#24011,#19375,#19376);
#17329=AXIS2_PLACEMENT_3D('',#24018,#19377,#19378);
#17330=AXIS2_PLACEMENT_3D('',#24027,#19379,#19380);
#17331=AXIS2_PLACEMENT_3D('',#24042,#19384,#19385);
#17332=AXIS2_PLACEMENT_3D('',#24044,#19386,#19387);
#17333=AXIS2_PLACEMENT_3D('',#24047,#19389,#19390);
#17334=AXIS2_PLACEMENT_3D('',#24048,#19391,#19392);
#17335=AXIS2_PLACEMENT_3D('',#24055,#19393,#19394);
#17336=AXIS2_PLACEMENT_3D('',#24064,#19395,#19396);
#17337=AXIS2_PLACEMENT_3D('',#24068,#19399,#19400);
#17338=AXIS2_PLACEMENT_3D('',#24070,#19401,#19402);
#17339=AXIS2_PLACEMENT_3D('',#24078,#19404,#19405);
#17340=AXIS2_PLACEMENT_3D('',#24079,#19406,#19407);
#17341=AXIS2_PLACEMENT_3D('',#24094,#19411,#19412);
#17342=AXIS2_PLACEMENT_3D('',#24096,#19413,#19414);
#17343=AXIS2_PLACEMENT_3D('',#24107,#19415,#19416);
#17344=AXIS2_PLACEMENT_3D('',#24112,#19417,#19418);
#17345=AXIS2_PLACEMENT_3D('',#24114,#19419,#19420);
#17346=AXIS2_PLACEMENT_3D('',#24116,#19422,#19423);
#17347=AXIS2_PLACEMENT_3D('',#24131,#19427,#19428);
#17348=AXIS2_PLACEMENT_3D('',#24132,#19429,#19430);
#17349=AXIS2_PLACEMENT_3D('',#24133,#19431,#19432);
#17350=AXIS2_PLACEMENT_3D('',#24134,#19433,#19434);
#17351=AXIS2_PLACEMENT_3D('',#24140,#19435,#19436);
#17352=AXIS2_PLACEMENT_3D('',#24141,#19437,#19438);
#17353=AXIS2_PLACEMENT_3D('',#24156,#19442,#19443);
#17354=AXIS2_PLACEMENT_3D('',#24158,#19444,#19445);
#17355=AXIS2_PLACEMENT_3D('',#24169,#19446,#19447);
#17356=AXIS2_PLACEMENT_3D('',#24174,#19448,#19449);
#17357=AXIS2_PLACEMENT_3D('',#24176,#19450,#19451);
#17358=AXIS2_PLACEMENT_3D('',#24178,#19453,#19454);
#17359=AXIS2_PLACEMENT_3D('',#24186,#19457,#19458);
#17360=AXIS2_PLACEMENT_3D('',#24194,#19461,#19462);
#17361=AXIS2_PLACEMENT_3D('',#24205,#19466,#19467);
#17362=AXIS2_PLACEMENT_3D('',#24212,#19468,#19469);
#17363=AXIS2_PLACEMENT_3D('',#24220,#19471,#19472);
#17364=AXIS2_PLACEMENT_3D('',#24221,#19473,#19474);
#17365=AXIS2_PLACEMENT_3D('',#24223,#19475,#19476);
#17366=AXIS2_PLACEMENT_3D('',#24234,#19477,#19478);
#17367=AXIS2_PLACEMENT_3D('',#24235,#19479,#19480);
#17368=AXIS2_PLACEMENT_3D('',#24250,#19484,#19485);
#17369=AXIS2_PLACEMENT_3D('',#24252,#19486,#19487);
#17370=AXIS2_PLACEMENT_3D('',#24255,#19489,#19490);
#17371=AXIS2_PLACEMENT_3D('',#24256,#19491,#19492);
#17372=AXIS2_PLACEMENT_3D('',#24263,#19493,#19494);
#17373=AXIS2_PLACEMENT_3D('',#24273,#19495,#19496);
#17374=AXIS2_PLACEMENT_3D('',#24288,#19500,#19501);
#17375=AXIS2_PLACEMENT_3D('',#24290,#19502,#19503);
#17376=AXIS2_PLACEMENT_3D('',#24301,#19504,#19505);
#17377=AXIS2_PLACEMENT_3D('',#24306,#19506,#19507);
#17378=AXIS2_PLACEMENT_3D('',#24308,#19508,#19509);
#17379=AXIS2_PLACEMENT_3D('',#24310,#19511,#19512);
#17380=AXIS2_PLACEMENT_3D('',#24318,#19515,#19516);
#17381=AXIS2_PLACEMENT_3D('',#24333,#19520,#19521);
#17382=AXIS2_PLACEMENT_3D('',#24335,#19522,#19523);
#17383=AXIS2_PLACEMENT_3D('',#24346,#19524,#19525);
#17384=AXIS2_PLACEMENT_3D('',#24351,#19526,#19527);
#17385=AXIS2_PLACEMENT_3D('',#24353,#19528,#19529);
#17386=AXIS2_PLACEMENT_3D('',#24355,#19531,#19532);
#17387=AXIS2_PLACEMENT_3D('',#24363,#19535,#19536);
#17388=AXIS2_PLACEMENT_3D('',#24378,#19540,#19541);
#17389=AXIS2_PLACEMENT_3D('',#24380,#19542,#19543);
#17390=AXIS2_PLACEMENT_3D('',#24391,#19544,#19545);
#17391=AXIS2_PLACEMENT_3D('',#24396,#19546,#19547);
#17392=AXIS2_PLACEMENT_3D('',#24398,#19548,#19549);
#17393=AXIS2_PLACEMENT_3D('',#24400,#19551,#19552);
#17394=AXIS2_PLACEMENT_3D('',#24408,#19555,#19556);
#17395=AXIS2_PLACEMENT_3D('',#24423,#19560,#19561);
#17396=AXIS2_PLACEMENT_3D('',#24425,#19562,#19563);
#17397=AXIS2_PLACEMENT_3D('',#24436,#19564,#19565);
#17398=AXIS2_PLACEMENT_3D('',#24441,#19566,#19567);
#17399=AXIS2_PLACEMENT_3D('',#24443,#19568,#19569);
#17400=AXIS2_PLACEMENT_3D('',#24445,#19571,#19572);
#17401=AXIS2_PLACEMENT_3D('',#24453,#19575,#19576);
#17402=AXIS2_PLACEMENT_3D('',#24468,#19580,#19581);
#17403=AXIS2_PLACEMENT_3D('',#24470,#19582,#19583);
#17404=AXIS2_PLACEMENT_3D('',#24481,#19584,#19585);
#17405=AXIS2_PLACEMENT_3D('',#24486,#19586,#19587);
#17406=AXIS2_PLACEMENT_3D('',#24488,#19588,#19589);
#17407=AXIS2_PLACEMENT_3D('',#24490,#19591,#19592);
#17408=AXIS2_PLACEMENT_3D('',#24498,#19595,#19596);
#17409=AXIS2_PLACEMENT_3D('',#24513,#19600,#19601);
#17410=AXIS2_PLACEMENT_3D('',#24515,#19602,#19603);
#17411=AXIS2_PLACEMENT_3D('',#24526,#19604,#19605);
#17412=AXIS2_PLACEMENT_3D('',#24531,#19606,#19607);
#17413=AXIS2_PLACEMENT_3D('',#24533,#19608,#19609);
#17414=AXIS2_PLACEMENT_3D('',#24535,#19611,#19612);
#17415=AXIS2_PLACEMENT_3D('',#24543,#19615,#19616);
#17416=AXIS2_PLACEMENT_3D('',#24558,#19620,#19621);
#17417=AXIS2_PLACEMENT_3D('',#24560,#19622,#19623);
#17418=AXIS2_PLACEMENT_3D('',#24571,#19624,#19625);
#17419=AXIS2_PLACEMENT_3D('',#24576,#19626,#19627);
#17420=AXIS2_PLACEMENT_3D('',#24578,#19628,#19629);
#17421=AXIS2_PLACEMENT_3D('',#24580,#19631,#19632);
#17422=AXIS2_PLACEMENT_3D('',#24588,#19635,#19636);
#17423=AXIS2_PLACEMENT_3D('',#24603,#19640,#19641);
#17424=AXIS2_PLACEMENT_3D('',#24605,#19642,#19643);
#17425=AXIS2_PLACEMENT_3D('',#24616,#19644,#19645);
#17426=AXIS2_PLACEMENT_3D('',#24621,#19646,#19647);
#17427=AXIS2_PLACEMENT_3D('',#24623,#19648,#19649);
#17428=AXIS2_PLACEMENT_3D('',#24625,#19651,#19652);
#17429=AXIS2_PLACEMENT_3D('',#24633,#19655,#19656);
#17430=AXIS2_PLACEMENT_3D('',#24635,#19657,#19658);
#17431=AXIS2_PLACEMENT_3D('',#24647,#19659,#19660);
#17432=AXIS2_PLACEMENT_3D('',#24648,#19661,#19662);
#17433=AXIS2_PLACEMENT_3D('',#24649,#19663,#19664);
#17434=AXIS2_PLACEMENT_3D('',#24650,#19665,#19666);
#17435=AXIS2_PLACEMENT_3D('',#24651,#19667,#19668);
#17436=AXIS2_PLACEMENT_3D('',#24652,#19669,#19670);
#17437=AXIS2_PLACEMENT_3D('',#24653,#19671,#19672);
#17438=AXIS2_PLACEMENT_3D('',#24654,#19673,#19674);
#17439=AXIS2_PLACEMENT_3D('',#24656,#19675,#19676);
#17440=AXIS2_PLACEMENT_3D('',#24666,#19677,#19678);
#17441=AXIS2_PLACEMENT_3D('',#24667,#19679,#19680);
#17442=AXIS2_PLACEMENT_3D('',#24669,#19681,#19682);
#17443=AXIS2_PLACEMENT_3D('',#24671,#19683,#19684);
#17444=AXIS2_PLACEMENT_3D('',#24673,#19685,#19686);
#17445=AXIS2_PLACEMENT_3D('',#24675,#19687,#19688);
#17446=AXIS2_PLACEMENT_3D('',#24677,#19689,#19690);
#17447=AXIS2_PLACEMENT_3D('',#24679,#19691,#19692);
#17448=AXIS2_PLACEMENT_3D('',#24681,#19693,#19694);
#17449=AXIS2_PLACEMENT_3D('',#24683,#19695,#19696);
#17450=AXIS2_PLACEMENT_3D('',#24685,#19697,#19698);
#17451=AXIS2_PLACEMENT_3D('',#24687,#19699,#19700);
#17452=AXIS2_PLACEMENT_3D('',#24689,#19701,#19702);
#17453=AXIS2_PLACEMENT_3D('',#24690,#19703,#19704);
#17454=AXIS2_PLACEMENT_3D('',#24691,#19705,#19706);
#17455=AXIS2_PLACEMENT_3D('',#24692,#19707,#19708);
#17456=AXIS2_PLACEMENT_3D('',#24693,#19709,#19710);
#17457=AXIS2_PLACEMENT_3D('',#24694,#19711,#19712);
#17458=AXIS2_PLACEMENT_3D('',#24695,#19713,#19714);
#17459=AXIS2_PLACEMENT_3D('',#24696,#19715,#19716);
#17460=AXIS2_PLACEMENT_3D('',#24697,#19717,#19718);
#17461=AXIS2_PLACEMENT_3D('',#24698,#19719,#19720);
#17462=AXIS2_PLACEMENT_3D('',#24699,#19721,#19722);
#17463=AXIS2_PLACEMENT_3D('',#24701,#19723,#19724);
#17464=AXIS2_PLACEMENT_3D('',#24703,#19725,#19726);
#17465=AXIS2_PLACEMENT_3D('',#24705,#19727,#19728);
#17466=AXIS2_PLACEMENT_3D('',#24707,#19729,#19730);
#17467=AXIS2_PLACEMENT_3D('',#24709,#19731,#19732);
#17468=AXIS2_PLACEMENT_3D('',#24711,#19733,#19734);
#17469=AXIS2_PLACEMENT_3D('',#24713,#19735,#19736);
#17470=AXIS2_PLACEMENT_3D('',#24715,#19737,#19738);
#17471=AXIS2_PLACEMENT_3D('',#24717,#19739,#19740);
#17472=AXIS2_PLACEMENT_3D('',#24719,#19741,#19742);
#17473=AXIS2_PLACEMENT_3D('',#24721,#19743,#19744);
#17474=AXIS2_PLACEMENT_3D('',#24723,#19745,#19746);
#17475=AXIS2_PLACEMENT_3D('',#24725,#19747,#19748);
#17476=AXIS2_PLACEMENT_3D('',#24727,#19749,#19750);
#17477=AXIS2_PLACEMENT_3D('',#24729,#19751,#19752);
#17478=AXIS2_PLACEMENT_3D('',#24731,#19753,#19754);
#17479=AXIS2_PLACEMENT_3D('',#24733,#19755,#19756);
#17480=AXIS2_PLACEMENT_3D('',#24734,#19757,#19758);
#17481=AXIS2_PLACEMENT_3D('',#24736,#19759,#19760);
#17482=AXIS2_PLACEMENT_3D('',#24738,#19761,#19762);
#17483=AXIS2_PLACEMENT_3D('',#24740,#19763,#19764);
#17484=AXIS2_PLACEMENT_3D('',#24742,#19765,#19766);
#17485=AXIS2_PLACEMENT_3D('',#24744,#19767,#19768);
#17486=AXIS2_PLACEMENT_3D('',#24746,#19769,#19770);
#17487=AXIS2_PLACEMENT_3D('',#24748,#19771,#19772);
#17488=AXIS2_PLACEMENT_3D('',#24750,#19773,#19774);
#17489=AXIS2_PLACEMENT_3D('',#24752,#19775,#19776);
#17490=AXIS2_PLACEMENT_3D('',#24754,#19777,#19778);
#17491=AXIS2_PLACEMENT_3D('',#24756,#19779,#19780);
#17492=AXIS2_PLACEMENT_3D('',#24758,#19781,#19782);
#17493=AXIS2_PLACEMENT_3D('',#24760,#19783,#19784);
#17494=AXIS2_PLACEMENT_3D('',#24762,#19785,#19786);
#17495=AXIS2_PLACEMENT_3D('',#24764,#19787,#19788);
#17496=AXIS2_PLACEMENT_3D('',#24766,#19789,#19790);
#17497=AXIS2_PLACEMENT_3D('',#24768,#19791,#19792);
#17498=AXIS2_PLACEMENT_3D('',#24770,#19793,#19794);
#17499=AXIS2_PLACEMENT_3D('',#24772,#19795,#19796);
#17500=AXIS2_PLACEMENT_3D('',#24774,#19797,#19798);
#17501=AXIS2_PLACEMENT_3D('',#24776,#19799,#19800);
#17502=AXIS2_PLACEMENT_3D('',#24778,#19801,#19802);
#17503=AXIS2_PLACEMENT_3D('',#24780,#19803,#19804);
#17504=AXIS2_PLACEMENT_3D('',#24782,#19805,#19806);
#17505=AXIS2_PLACEMENT_3D('',#24784,#19807,#19808);
#17506=AXIS2_PLACEMENT_3D('',#24786,#19809,#19810);
#17507=AXIS2_PLACEMENT_3D('',#24788,#19811,#19812);
#17508=AXIS2_PLACEMENT_3D('',#24790,#19813,#19814);
#17509=AXIS2_PLACEMENT_3D('',#24792,#19815,#19816);
#17510=AXIS2_PLACEMENT_3D('',#24794,#19817,#19818);
#17511=AXIS2_PLACEMENT_3D('',#24796,#19819,#19820);
#17512=AXIS2_PLACEMENT_3D('',#24798,#19821,#19822);
#17513=AXIS2_PLACEMENT_3D('',#24800,#19823,#19824);
#17514=AXIS2_PLACEMENT_3D('',#24802,#19825,#19826);
#17515=AXIS2_PLACEMENT_3D('',#24804,#19827,#19828);
#17516=AXIS2_PLACEMENT_3D('',#24806,#19829,#19830);
#17517=AXIS2_PLACEMENT_3D('',#24808,#19831,#19832);
#17518=AXIS2_PLACEMENT_3D('',#24810,#19833,#19834);
#17519=AXIS2_PLACEMENT_3D('',#24812,#19835,#19836);
#17520=AXIS2_PLACEMENT_3D('',#24814,#19837,#19838);
#17521=AXIS2_PLACEMENT_3D('',#24816,#19839,#19840);
#17522=AXIS2_PLACEMENT_3D('',#24818,#19841,#19842);
#17523=AXIS2_PLACEMENT_3D('',#24820,#19843,#19844);
#17524=AXIS2_PLACEMENT_3D('',#24822,#19845,#19846);
#17525=AXIS2_PLACEMENT_3D('',#24824,#19847,#19848);
#17526=AXIS2_PLACEMENT_3D('',#24826,#19849,#19850);
#17527=AXIS2_PLACEMENT_3D('',#24828,#19851,#19852);
#17528=AXIS2_PLACEMENT_3D('',#24830,#19853,#19854);
#17529=AXIS2_PLACEMENT_3D('',#24832,#19855,#19856);
#17530=AXIS2_PLACEMENT_3D('',#24834,#19857,#19858);
#17531=AXIS2_PLACEMENT_3D('',#24836,#19859,#19860);
#17532=AXIS2_PLACEMENT_3D('',#24838,#19861,#19862);
#17533=AXIS2_PLACEMENT_3D('',#24840,#19863,#19864);
#17534=AXIS2_PLACEMENT_3D('',#24842,#19865,#19866);
#17535=AXIS2_PLACEMENT_3D('',#24844,#19867,#19868);
#17536=AXIS2_PLACEMENT_3D('',#24846,#19869,#19870);
#17537=AXIS2_PLACEMENT_3D('',#24848,#19871,#19872);
#17538=AXIS2_PLACEMENT_3D('',#24850,#19873,#19874);
#17539=AXIS2_PLACEMENT_3D('',#24852,#19875,#19876);
#17540=AXIS2_PLACEMENT_3D('',#24854,#19877,#19878);
#17541=AXIS2_PLACEMENT_3D('',#24856,#19879,#19880);
#17542=AXIS2_PLACEMENT_3D('',#24858,#19881,#19882);
#17543=AXIS2_PLACEMENT_3D('',#24860,#19883,#19884);
#17544=AXIS2_PLACEMENT_3D('',#24862,#19885,#19886);
#17545=AXIS2_PLACEMENT_3D('',#24864,#19887,#19888);
#17546=AXIS2_PLACEMENT_3D('',#24866,#19889,#19890);
#17547=AXIS2_PLACEMENT_3D('',#24868,#19891,#19892);
#17548=AXIS2_PLACEMENT_3D('',#24870,#19893,#19894);
#17549=AXIS2_PLACEMENT_3D('',#24872,#19895,#19896);
#17550=AXIS2_PLACEMENT_3D('',#24874,#19897,#19898);
#17551=AXIS2_PLACEMENT_3D('',#24876,#19899,#19900);
#17552=AXIS2_PLACEMENT_3D('',#24878,#19901,#19902);
#17553=AXIS2_PLACEMENT_3D('',#24880,#19903,#19904);
#17554=AXIS2_PLACEMENT_3D('',#24882,#19905,#19906);
#17555=AXIS2_PLACEMENT_3D('',#24884,#19907,#19908);
#17556=AXIS2_PLACEMENT_3D('',#24886,#19909,#19910);
#17557=AXIS2_PLACEMENT_3D('',#24888,#19911,#19912);
#17558=AXIS2_PLACEMENT_3D('',#24890,#19913,#19914);
#17559=AXIS2_PLACEMENT_3D('',#24892,#19915,#19916);
#17560=AXIS2_PLACEMENT_3D('',#24894,#19917,#19918);
#17561=AXIS2_PLACEMENT_3D('',#24896,#19919,#19920);
#17562=AXIS2_PLACEMENT_3D('',#24898,#19921,#19922);
#17563=AXIS2_PLACEMENT_3D('',#24900,#19923,#19924);
#17564=AXIS2_PLACEMENT_3D('',#24902,#19925,#19926);
#17565=AXIS2_PLACEMENT_3D('',#24904,#19927,#19928);
#17566=AXIS2_PLACEMENT_3D('',#24906,#19929,#19930);
#17567=AXIS2_PLACEMENT_3D('',#24908,#19931,#19932);
#17568=AXIS2_PLACEMENT_3D('',#24910,#19933,#19934);
#17569=AXIS2_PLACEMENT_3D('',#24912,#19935,#19936);
#17570=AXIS2_PLACEMENT_3D('',#24914,#19937,#19938);
#17571=AXIS2_PLACEMENT_3D('',#24916,#19939,#19940);
#17572=AXIS2_PLACEMENT_3D('',#24918,#19941,#19942);
#17573=AXIS2_PLACEMENT_3D('',#24920,#19943,#19944);
#17574=AXIS2_PLACEMENT_3D('',#24922,#19945,#19946);
#17575=AXIS2_PLACEMENT_3D('',#24924,#19947,#19948);
#17576=AXIS2_PLACEMENT_3D('',#24926,#19949,#19950);
#17577=AXIS2_PLACEMENT_3D('',#24928,#19951,#19952);
#17578=AXIS2_PLACEMENT_3D('',#24930,#19953,#19954);
#17579=AXIS2_PLACEMENT_3D('',#24932,#19955,#19956);
#17580=AXIS2_PLACEMENT_3D('',#24934,#19957,#19958);
#17581=AXIS2_PLACEMENT_3D('',#24936,#19959,#19960);
#17582=AXIS2_PLACEMENT_3D('',#24938,#19961,#19962);
#17583=AXIS2_PLACEMENT_3D('',#24940,#19963,#19964);
#17584=AXIS2_PLACEMENT_3D('',#24942,#19965,#19966);
#17585=AXIS2_PLACEMENT_3D('',#24944,#19967,#19968);
#17586=AXIS2_PLACEMENT_3D('',#24946,#19969,#19970);
#17587=AXIS2_PLACEMENT_3D('',#24948,#19971,#19972);
#17588=AXIS2_PLACEMENT_3D('',#24950,#19973,#19974);
#17589=AXIS2_PLACEMENT_3D('',#24952,#19975,#19976);
#17590=AXIS2_PLACEMENT_3D('',#24954,#19977,#19978);
#17591=AXIS2_PLACEMENT_3D('',#24956,#19979,#19980);
#17592=AXIS2_PLACEMENT_3D('',#24958,#19981,#19982);
#17593=AXIS2_PLACEMENT_3D('',#24960,#19983,#19984);
#17594=AXIS2_PLACEMENT_3D('',#24962,#19985,#19986);
#17595=AXIS2_PLACEMENT_3D('',#24964,#19987,#19988);
#17596=AXIS2_PLACEMENT_3D('',#24966,#19989,#19990);
#17597=AXIS2_PLACEMENT_3D('',#24968,#19991,#19992);
#17598=AXIS2_PLACEMENT_3D('',#24970,#19993,#19994);
#17599=AXIS2_PLACEMENT_3D('',#24972,#19995,#19996);
#17600=AXIS2_PLACEMENT_3D('',#24973,#19997,#19998);
#17601=AXIS2_PLACEMENT_3D('',#24975,#19999,#20000);
#17602=AXIS2_PLACEMENT_3D('',#24976,#20001,#20002);
#17603=AXIS2_PLACEMENT_3D('',#24980,#20004,#20005);
#17604=AXIS2_PLACEMENT_3D('',#24987,#20007,#20008);
#17605=AXIS2_PLACEMENT_3D('',#24991,#20011,#20012);
#17606=AXIS2_PLACEMENT_3D('',#25006,#20016,#20017);
#17607=AXIS2_PLACEMENT_3D('',#25008,#20018,#20019);
#17608=AXIS2_PLACEMENT_3D('',#25021,#20020,#20021);
#17609=AXIS2_PLACEMENT_3D('',#25023,#20022,#20023);
#17610=AXIS2_PLACEMENT_3D('',#25025,#20025,#20026);
#17611=AXIS2_PLACEMENT_3D('',#25033,#20029,#20030);
#17612=AXIS2_PLACEMENT_3D('',#25048,#20034,#20035);
#17613=AXIS2_PLACEMENT_3D('',#25050,#20036,#20037);
#17614=AXIS2_PLACEMENT_3D('',#25063,#20038,#20039);
#17615=AXIS2_PLACEMENT_3D('',#25065,#20040,#20041);
#17616=AXIS2_PLACEMENT_3D('',#25067,#20043,#20044);
#17617=AXIS2_PLACEMENT_3D('',#25075,#20047,#20048);
#17618=AXIS2_PLACEMENT_3D('',#25090,#20052,#20053);
#17619=AXIS2_PLACEMENT_3D('',#25092,#20054,#20055);
#17620=AXIS2_PLACEMENT_3D('',#25105,#20056,#20057);
#17621=AXIS2_PLACEMENT_3D('',#25107,#20058,#20059);
#17622=AXIS2_PLACEMENT_3D('',#25109,#20061,#20062);
#17623=AXIS2_PLACEMENT_3D('',#25117,#20065,#20066);
#17624=AXIS2_PLACEMENT_3D('',#25119,#20067,#20068);
#17625=AXIS2_PLACEMENT_3D('',#25122,#20070,#20071);
#17626=AXIS2_PLACEMENT_3D('',#25123,#20072,#20073);
#17627=AXIS2_PLACEMENT_3D('',#25127,#20074,#20075);
#17628=AXIS2_PLACEMENT_3D('',#25129,#20077,#20078);
#17629=AXIS2_PLACEMENT_3D('',#25140,#20082,#20083);
#17630=AXIS2_PLACEMENT_3D('',#25142,#20084,#20085);
#17631=AXIS2_PLACEMENT_3D('',#25155,#20086,#20087);
#17632=AXIS2_PLACEMENT_3D('',#25157,#20088,#20089);
#17633=AXIS2_PLACEMENT_3D('',#25159,#20091,#20092);
#17634=AXIS2_PLACEMENT_3D('',#25167,#20095,#20096);
#17635=AXIS2_PLACEMENT_3D('',#25182,#20100,#20101);
#17636=AXIS2_PLACEMENT_3D('',#25184,#20102,#20103);
#17637=AXIS2_PLACEMENT_3D('',#25197,#20104,#20105);
#17638=AXIS2_PLACEMENT_3D('',#25199,#20106,#20107);
#17639=AXIS2_PLACEMENT_3D('',#25201,#20109,#20110);
#17640=AXIS2_PLACEMENT_3D('',#25209,#20113,#20114);
#17641=AXIS2_PLACEMENT_3D('',#25224,#20118,#20119);
#17642=AXIS2_PLACEMENT_3D('',#25226,#20120,#20121);
#17643=AXIS2_PLACEMENT_3D('',#25239,#20122,#20123);
#17644=AXIS2_PLACEMENT_3D('',#25241,#20124,#20125);
#17645=AXIS2_PLACEMENT_3D('',#25243,#20127,#20128);
#17646=AXIS2_PLACEMENT_3D('',#25251,#20131,#20132);
#17647=AXIS2_PLACEMENT_3D('',#25266,#20136,#20137);
#17648=AXIS2_PLACEMENT_3D('',#25268,#20138,#20139);
#17649=AXIS2_PLACEMENT_3D('',#25281,#20140,#20141);
#17650=AXIS2_PLACEMENT_3D('',#25283,#20142,#20143);
#17651=AXIS2_PLACEMENT_3D('',#25285,#20145,#20146);
#17652=AXIS2_PLACEMENT_3D('',#25293,#20149,#20150);
#17653=AXIS2_PLACEMENT_3D('',#25308,#20154,#20155);
#17654=AXIS2_PLACEMENT_3D('',#25310,#20156,#20157);
#17655=AXIS2_PLACEMENT_3D('',#25323,#20158,#20159);
#17656=AXIS2_PLACEMENT_3D('',#25325,#20160,#20161);
#17657=AXIS2_PLACEMENT_3D('',#25327,#20163,#20164);
#17658=AXIS2_PLACEMENT_3D('',#25335,#20167,#20168);
#17659=AXIS2_PLACEMENT_3D('',#25350,#20172,#20173);
#17660=AXIS2_PLACEMENT_3D('',#25352,#20174,#20175);
#17661=AXIS2_PLACEMENT_3D('',#25365,#20176,#20177);
#17662=AXIS2_PLACEMENT_3D('',#25367,#20178,#20179);
#17663=AXIS2_PLACEMENT_3D('',#25369,#20181,#20182);
#17664=AXIS2_PLACEMENT_3D('',#25381,#20186,#20187);
#17665=AXIS2_PLACEMENT_3D('',#25386,#20188,#20189);
#17666=AXIS2_PLACEMENT_3D('',#25387,#20190,#20191);
#17667=AXIS2_PLACEMENT_3D('',#25388,#20192,#20193);
#17668=AXIS2_PLACEMENT_3D('',#25389,#20194,#20195);
#17669=AXIS2_PLACEMENT_3D('',#25390,#20196,#20197);
#17670=AXIS2_PLACEMENT_3D('',#25391,#20198,#20199);
#17671=AXIS2_PLACEMENT_3D('',#25392,#20200,#20201);
#17672=AXIS2_PLACEMENT_3D('',#25393,#20202,#20203);
#17673=AXIS2_PLACEMENT_3D('',#25394,#20204,#20205);
#17674=AXIS2_PLACEMENT_3D('',#25395,#20206,#20207);
#17675=AXIS2_PLACEMENT_3D('',#25396,#20208,#20209);
#17676=AXIS2_PLACEMENT_3D('',#25397,#20210,#20211);
#17677=AXIS2_PLACEMENT_3D('',#25401,#20214,#20215);
#17678=AXIS2_PLACEMENT_3D('',#25402,#20216,#20217);
#17679=AXIS2_PLACEMENT_3D('',#25403,#20218,#20219);
#17680=AXIS2_PLACEMENT_3D('',#25404,#20220,#20221);
#17681=AXIS2_PLACEMENT_3D('',#25405,#20222,#20223);
#17682=AXIS2_PLACEMENT_3D('',#25406,#20224,#20225);
#17683=AXIS2_PLACEMENT_3D('',#25407,#20226,#20227);
#17684=AXIS2_PLACEMENT_3D('',#25408,#20228,#20229);
#17685=AXIS2_PLACEMENT_3D('',#25409,#20230,#20231);
#17686=AXIS2_PLACEMENT_3D('',#25410,#20232,#20233);
#17687=AXIS2_PLACEMENT_3D('',#25411,#20234,#20235);
#17688=AXIS2_PLACEMENT_3D('',#25412,#20236,#20237);
#17689=AXIS2_PLACEMENT_3D('',#25413,#20238,#20239);
#17690=AXIS2_PLACEMENT_3D('',#25414,#20240,#20241);
#17691=AXIS2_PLACEMENT_3D('',#25415,#20242,#20243);
#17692=AXIS2_PLACEMENT_3D('',#25416,#20244,#20245);
#17693=AXIS2_PLACEMENT_3D('',#25417,#20246,#20247);
#17694=AXIS2_PLACEMENT_3D('',#25418,#20248,#20249);
#17695=AXIS2_PLACEMENT_3D('',#25419,#20250,#20251);
#17696=AXIS2_PLACEMENT_3D('',#25420,#20252,#20253);
#17697=AXIS2_PLACEMENT_3D('',#25421,#20254,#20255);
#17698=AXIS2_PLACEMENT_3D('',#25422,#20256,#20257);
#17699=AXIS2_PLACEMENT_3D('',#25423,#20258,#20259);
#17700=AXIS2_PLACEMENT_3D('',#25438,#20263,#20264);
#17701=AXIS2_PLACEMENT_3D('',#25440,#20265,#20266);
#17702=AXIS2_PLACEMENT_3D('',#25453,#20267,#20268);
#17703=AXIS2_PLACEMENT_3D('',#25455,#20269,#20270);
#17704=AXIS2_PLACEMENT_3D('',#25457,#20272,#20273);
#17705=AXIS2_PLACEMENT_3D('',#25465,#20276,#20277);
#17706=AXIS2_PLACEMENT_3D('',#25467,#20278,#20279);
#17707=AXIS2_PLACEMENT_3D('',#25476,#20280,#20281);
#17708=AXIS2_PLACEMENT_3D('',#25486,#20285,#20286);
#17709=AXIS2_PLACEMENT_3D('',#25488,#20287,#20288);
#17710=AXIS2_PLACEMENT_3D('',#25497,#20289,#20290);
#17711=AXIS2_PLACEMENT_3D('',#25499,#20291,#20292);
#17712=AXIS2_PLACEMENT_3D('',#25501,#20294,#20295);
#17713=AXIS2_PLACEMENT_3D('',#25509,#20298,#20299);
#17714=AXIS2_PLACEMENT_3D('',#25524,#20303,#20304);
#17715=AXIS2_PLACEMENT_3D('',#25526,#20305,#20306);
#17716=AXIS2_PLACEMENT_3D('',#25539,#20307,#20308);
#17717=AXIS2_PLACEMENT_3D('',#25541,#20309,#20310);
#17718=AXIS2_PLACEMENT_3D('',#25543,#20312,#20313);
#17719=AXIS2_PLACEMENT_3D('',#25551,#20316,#20317);
#17720=AXIS2_PLACEMENT_3D('',#25566,#20321,#20322);
#17721=AXIS2_PLACEMENT_3D('',#25568,#20323,#20324);
#17722=AXIS2_PLACEMENT_3D('',#25581,#20325,#20326);
#17723=AXIS2_PLACEMENT_3D('',#25583,#20327,#20328);
#17724=AXIS2_PLACEMENT_3D('',#25585,#20330,#20331);
#17725=AXIS2_PLACEMENT_3D('',#25596,#20335,#20336);
#17726=AXIS2_PLACEMENT_3D('',#25598,#20337,#20338);
#17727=AXIS2_PLACEMENT_3D('',#25601,#20340,#20341);
#17728=AXIS2_PLACEMENT_3D('',#25602,#20342,#20343);
#17729=AXIS2_PLACEMENT_3D('',#25610,#20344,#20345);
#17730=AXIS2_PLACEMENT_3D('',#25612,#20347,#20348);
#17731=AXIS2_PLACEMENT_3D('',#25623,#20352,#20353);
#17732=AXIS2_PLACEMENT_3D('',#25625,#20354,#20355);
#17733=AXIS2_PLACEMENT_3D('',#25638,#20356,#20357);
#17734=AXIS2_PLACEMENT_3D('',#25640,#20358,#20359);
#17735=AXIS2_PLACEMENT_3D('',#25642,#20361,#20362);
#17736=AXIS2_PLACEMENT_3D('',#25650,#20365,#20366);
#17737=AXIS2_PLACEMENT_3D('',#25665,#20370,#20371);
#17738=AXIS2_PLACEMENT_3D('',#25667,#20372,#20373);
#17739=AXIS2_PLACEMENT_3D('',#25680,#20374,#20375);
#17740=AXIS2_PLACEMENT_3D('',#25682,#20376,#20377);
#17741=AXIS2_PLACEMENT_3D('',#25684,#20379,#20380);
#17742=AXIS2_PLACEMENT_3D('',#25692,#20383,#20384);
#17743=AXIS2_PLACEMENT_3D('',#25707,#20388,#20389);
#17744=AXIS2_PLACEMENT_3D('',#25709,#20390,#20391);
#17745=AXIS2_PLACEMENT_3D('',#25722,#20392,#20393);
#17746=AXIS2_PLACEMENT_3D('',#25724,#20394,#20395);
#17747=AXIS2_PLACEMENT_3D('',#25726,#20397,#20398);
#17748=AXIS2_PLACEMENT_3D('',#25734,#20401,#20402);
#17749=AXIS2_PLACEMENT_3D('',#25749,#20406,#20407);
#17750=AXIS2_PLACEMENT_3D('',#25751,#20408,#20409);
#17751=AXIS2_PLACEMENT_3D('',#25764,#20410,#20411);
#17752=AXIS2_PLACEMENT_3D('',#25766,#20412,#20413);
#17753=AXIS2_PLACEMENT_3D('',#25768,#20415,#20416);
#17754=AXIS2_PLACEMENT_3D('',#25776,#20419,#20420);
#17755=AXIS2_PLACEMENT_3D('',#25791,#20424,#20425);
#17756=AXIS2_PLACEMENT_3D('',#25793,#20426,#20427);
#17757=AXIS2_PLACEMENT_3D('',#25806,#20428,#20429);
#17758=AXIS2_PLACEMENT_3D('',#25808,#20430,#20431);
#17759=AXIS2_PLACEMENT_3D('',#25810,#20433,#20434);
#17760=AXIS2_PLACEMENT_3D('',#25822,#20438,#20439);
#17761=AXIS2_PLACEMENT_3D('',#25827,#20440,#20441);
#17762=AXIS2_PLACEMENT_3D('',#25828,#20442,#20443);
#17763=AXIS2_PLACEMENT_3D('',#25829,#20444,#20445);
#17764=AXIS2_PLACEMENT_3D('',#25830,#20446,#20447);
#17765=AXIS2_PLACEMENT_3D('',#25831,#20448,#20449);
#17766=AXIS2_PLACEMENT_3D('',#25832,#20450,#20451);
#17767=AXIS2_PLACEMENT_3D('',#25833,#20452,#20453);
#17768=AXIS2_PLACEMENT_3D('',#25834,#20454,#20455);
#17769=AXIS2_PLACEMENT_3D('',#25835,#20456,#20457);
#17770=AXIS2_PLACEMENT_3D('',#25836,#20458,#20459);
#17771=AXIS2_PLACEMENT_3D('',#25837,#20460,#20461);
#17772=AXIS2_PLACEMENT_3D('',#25838,#20462,#20463);
#17773=AXIS2_PLACEMENT_3D('',#25839,#20464,#20465);
#17774=AXIS2_PLACEMENT_3D('',#25840,#20466,#20467);
#17775=AXIS2_PLACEMENT_3D('',#25844,#20470,#20471);
#17776=AXIS2_PLACEMENT_3D('',#25845,#20472,#20473);
#17777=AXIS2_PLACEMENT_3D('',#25846,#20474,#20475);
#17778=AXIS2_PLACEMENT_3D('',#25847,#20476,#20477);
#17779=AXIS2_PLACEMENT_3D('',#25848,#20478,#20479);
#17780=AXIS2_PLACEMENT_3D('',#25849,#20480,#20481);
#17781=AXIS2_PLACEMENT_3D('',#25850,#20482,#20483);
#17782=AXIS2_PLACEMENT_3D('',#25851,#20484,#20485);
#17783=AXIS2_PLACEMENT_3D('',#25852,#20486,#20487);
#17784=AXIS2_PLACEMENT_3D('',#25853,#20488,#20489);
#17785=AXIS2_PLACEMENT_3D('',#25854,#20490,#20491);
#17786=AXIS2_PLACEMENT_3D('',#25855,#20492,#20493);
#17787=AXIS2_PLACEMENT_3D('',#25856,#20494,#20495);
#17788=AXIS2_PLACEMENT_3D('',#25857,#20496,#20497);
#17789=AXIS2_PLACEMENT_3D('',#25858,#20498,#20499);
#17790=AXIS2_PLACEMENT_3D('',#25859,#20500,#20501);
#17791=AXIS2_PLACEMENT_3D('',#25860,#20502,#20503);
#17792=AXIS2_PLACEMENT_3D('',#25861,#20504,#20505);
#17793=AXIS2_PLACEMENT_3D('',#25862,#20506,#20507);
#17794=AXIS2_PLACEMENT_3D('',#25877,#20511,#20512);
#17795=AXIS2_PLACEMENT_3D('',#25879,#20513,#20514);
#17796=AXIS2_PLACEMENT_3D('',#25892,#20515,#20516);
#17797=AXIS2_PLACEMENT_3D('',#25894,#20517,#20518);
#17798=AXIS2_PLACEMENT_3D('',#25896,#20520,#20521);
#17799=AXIS2_PLACEMENT_3D('',#25904,#20524,#20525);
#17800=AXIS2_PLACEMENT_3D('',#25919,#20529,#20530);
#17801=AXIS2_PLACEMENT_3D('',#25921,#20531,#20532);
#17802=AXIS2_PLACEMENT_3D('',#25934,#20533,#20534);
#17803=AXIS2_PLACEMENT_3D('',#25936,#20535,#20536);
#17804=AXIS2_PLACEMENT_3D('',#25938,#20538,#20539);
#17805=AXIS2_PLACEMENT_3D('',#25946,#20542,#20543);
#17806=AXIS2_PLACEMENT_3D('',#25961,#20547,#20548);
#17807=AXIS2_PLACEMENT_3D('',#25963,#20549,#20550);
#17808=AXIS2_PLACEMENT_3D('',#25976,#20551,#20552);
#17809=AXIS2_PLACEMENT_3D('',#25978,#20553,#20554);
#17810=AXIS2_PLACEMENT_3D('',#25980,#20556,#20557);
#17811=AXIS2_PLACEMENT_3D('',#25988,#20560,#20561);
#17812=AXIS2_PLACEMENT_3D('',#26003,#20565,#20566);
#17813=AXIS2_PLACEMENT_3D('',#26005,#20567,#20568);
#17814=AXIS2_PLACEMENT_3D('',#26018,#20569,#20570);
#17815=AXIS2_PLACEMENT_3D('',#26020,#20571,#20572);
#17816=AXIS2_PLACEMENT_3D('',#26022,#20574,#20575);
#17817=AXIS2_PLACEMENT_3D('',#26030,#20578,#20579);
#17818=AXIS2_PLACEMENT_3D('',#26045,#20583,#20584);
#17819=AXIS2_PLACEMENT_3D('',#26047,#20585,#20586);
#17820=AXIS2_PLACEMENT_3D('',#26060,#20587,#20588);
#17821=AXIS2_PLACEMENT_3D('',#26062,#20589,#20590);
#17822=AXIS2_PLACEMENT_3D('',#26064,#20592,#20593);
#17823=AXIS2_PLACEMENT_3D('',#26075,#20597,#20598);
#17824=AXIS2_PLACEMENT_3D('',#26077,#20599,#20600);
#17825=AXIS2_PLACEMENT_3D('',#26080,#20602,#20603);
#17826=AXIS2_PLACEMENT_3D('',#26081,#20604,#20605);
#17827=AXIS2_PLACEMENT_3D('',#26089,#20606,#20607);
#17828=AXIS2_PLACEMENT_3D('',#26091,#20609,#20610);
#17829=AXIS2_PLACEMENT_3D('',#26102,#20614,#20615);
#17830=AXIS2_PLACEMENT_3D('',#26104,#20616,#20617);
#17831=AXIS2_PLACEMENT_3D('',#26117,#20618,#20619);
#17832=AXIS2_PLACEMENT_3D('',#26119,#20620,#20621);
#17833=AXIS2_PLACEMENT_3D('',#26121,#20623,#20624);
#17834=AXIS2_PLACEMENT_3D('',#26129,#20627,#20628);
#17835=AXIS2_PLACEMENT_3D('',#26144,#20632,#20633);
#17836=AXIS2_PLACEMENT_3D('',#26146,#20634,#20635);
#17837=AXIS2_PLACEMENT_3D('',#26159,#20636,#20637);
#17838=AXIS2_PLACEMENT_3D('',#26161,#20638,#20639);
#17839=AXIS2_PLACEMENT_3D('',#26163,#20641,#20642);
#17840=AXIS2_PLACEMENT_3D('',#26171,#20645,#20646);
#17841=AXIS2_PLACEMENT_3D('',#26186,#20650,#20651);
#17842=AXIS2_PLACEMENT_3D('',#26188,#20652,#20653);
#17843=AXIS2_PLACEMENT_3D('',#26201,#20654,#20655);
#17844=AXIS2_PLACEMENT_3D('',#26203,#20656,#20657);
#17845=AXIS2_PLACEMENT_3D('',#26205,#20659,#20660);
#17846=AXIS2_PLACEMENT_3D('',#26213,#20663,#20664);
#17847=AXIS2_PLACEMENT_3D('',#26228,#20668,#20669);
#17848=AXIS2_PLACEMENT_3D('',#26230,#20670,#20671);
#17849=AXIS2_PLACEMENT_3D('',#26243,#20672,#20673);
#17850=AXIS2_PLACEMENT_3D('',#26245,#20674,#20675);
#17851=AXIS2_PLACEMENT_3D('',#26247,#20677,#20678);
#17852=AXIS2_PLACEMENT_3D('',#26259,#20682,#20683);
#17853=AXIS2_PLACEMENT_3D('',#26264,#20684,#20685);
#17854=AXIS2_PLACEMENT_3D('',#26265,#20686,#20687);
#17855=AXIS2_PLACEMENT_3D('',#26266,#20688,#20689);
#17856=AXIS2_PLACEMENT_3D('',#26267,#20690,#20691);
#17857=AXIS2_PLACEMENT_3D('',#26268,#20692,#20693);
#17858=AXIS2_PLACEMENT_3D('',#26269,#20694,#20695);
#17859=AXIS2_PLACEMENT_3D('',#26270,#20696,#20697);
#17860=AXIS2_PLACEMENT_3D('',#26271,#20698,#20699);
#17861=AXIS2_PLACEMENT_3D('',#26272,#20700,#20701);
#17862=AXIS2_PLACEMENT_3D('',#26273,#20702,#20703);
#17863=AXIS2_PLACEMENT_3D('',#26274,#20704,#20705);
#17864=AXIS2_PLACEMENT_3D('',#26275,#20706,#20707);
#17865=AXIS2_PLACEMENT_3D('',#26276,#20708,#20709);
#17866=AXIS2_PLACEMENT_3D('',#26277,#20710,#20711);
#17867=AXIS2_PLACEMENT_3D('',#26278,#20712,#20713);
#17868=AXIS2_PLACEMENT_3D('',#26279,#20714,#20715);
#17869=AXIS2_PLACEMENT_3D('',#26280,#20716,#20717);
#17870=AXIS2_PLACEMENT_3D('',#26281,#20718,#20719);
#17871=AXIS2_PLACEMENT_3D('',#26282,#20720,#20721);
#17872=AXIS2_PLACEMENT_3D('',#26283,#20722,#20723);
#17873=AXIS2_PLACEMENT_3D('',#26287,#20726,#20727);
#17874=AXIS2_PLACEMENT_3D('',#26288,#20728,#20729);
#17875=AXIS2_PLACEMENT_3D('',#26289,#20730,#20731);
#17876=AXIS2_PLACEMENT_3D('',#26290,#20732,#20733);
#17877=AXIS2_PLACEMENT_3D('',#26291,#20734,#20735);
#17878=AXIS2_PLACEMENT_3D('',#26292,#20736,#20737);
#17879=AXIS2_PLACEMENT_3D('',#26293,#20738,#20739);
#17880=AXIS2_PLACEMENT_3D('',#26294,#20740,#20741);
#17881=AXIS2_PLACEMENT_3D('',#26295,#20742,#20743);
#17882=AXIS2_PLACEMENT_3D('',#26296,#20744,#20745);
#17883=AXIS2_PLACEMENT_3D('',#26297,#20746,#20747);
#17884=AXIS2_PLACEMENT_3D('',#26298,#20748,#20749);
#17885=AXIS2_PLACEMENT_3D('',#26299,#20750,#20751);
#17886=AXIS2_PLACEMENT_3D('',#26300,#20752,#20753);
#17887=AXIS2_PLACEMENT_3D('',#26301,#20754,#20755);
#17888=AXIS2_PLACEMENT_3D('',#26316,#20759,#20760);
#17889=AXIS2_PLACEMENT_3D('',#26318,#20761,#20762);
#17890=AXIS2_PLACEMENT_3D('',#26331,#20763,#20764);
#17891=AXIS2_PLACEMENT_3D('',#26333,#20765,#20766);
#17892=AXIS2_PLACEMENT_3D('',#26335,#20768,#20769);
#17893=AXIS2_PLACEMENT_3D('',#26343,#20772,#20773);
#17894=AXIS2_PLACEMENT_3D('',#26345,#20774,#20775);
#17895=AXIS2_PLACEMENT_3D('',#26354,#20776,#20777);
#17896=AXIS2_PLACEMENT_3D('',#26364,#20781,#20782);
#17897=AXIS2_PLACEMENT_3D('',#26366,#20783,#20784);
#17898=AXIS2_PLACEMENT_3D('',#26375,#20785,#20786);
#17899=AXIS2_PLACEMENT_3D('',#26377,#20787,#20788);
#17900=AXIS2_PLACEMENT_3D('',#26379,#20790,#20791);
#17901=AXIS2_PLACEMENT_3D('',#26387,#20794,#20795);
#17902=AXIS2_PLACEMENT_3D('',#26402,#20799,#20800);
#17903=AXIS2_PLACEMENT_3D('',#26404,#20801,#20802);
#17904=AXIS2_PLACEMENT_3D('',#26417,#20803,#20804);
#17905=AXIS2_PLACEMENT_3D('',#26419,#20805,#20806);
#17906=AXIS2_PLACEMENT_3D('',#26421,#20808,#20809);
#17907=AXIS2_PLACEMENT_3D('',#26429,#20812,#20813);
#17908=AXIS2_PLACEMENT_3D('',#26444,#20817,#20818);
#17909=AXIS2_PLACEMENT_3D('',#26446,#20819,#20820);
#17910=AXIS2_PLACEMENT_3D('',#26459,#20821,#20822);
#17911=AXIS2_PLACEMENT_3D('',#26461,#20823,#20824);
#17912=AXIS2_PLACEMENT_3D('',#26463,#20826,#20827);
#17913=AXIS2_PLACEMENT_3D('',#26471,#20830,#20831);
#17914=AXIS2_PLACEMENT_3D('',#26486,#20835,#20836);
#17915=AXIS2_PLACEMENT_3D('',#26488,#20837,#20838);
#17916=AXIS2_PLACEMENT_3D('',#26501,#20839,#20840);
#17917=AXIS2_PLACEMENT_3D('',#26503,#20841,#20842);
#17918=AXIS2_PLACEMENT_3D('',#26505,#20844,#20845);
#17919=AXIS2_PLACEMENT_3D('',#26513,#20848,#20849);
#17920=AXIS2_PLACEMENT_3D('',#26528,#20853,#20854);
#17921=AXIS2_PLACEMENT_3D('',#26530,#20855,#20856);
#17922=AXIS2_PLACEMENT_3D('',#26543,#20857,#20858);
#17923=AXIS2_PLACEMENT_3D('',#26545,#20859,#20860);
#17924=AXIS2_PLACEMENT_3D('',#26547,#20862,#20863);
#17925=AXIS2_PLACEMENT_3D('',#26558,#20867,#20868);
#17926=AXIS2_PLACEMENT_3D('',#26560,#20869,#20870);
#17927=AXIS2_PLACEMENT_3D('',#26563,#20872,#20873);
#17928=AXIS2_PLACEMENT_3D('',#26564,#20874,#20875);
#17929=AXIS2_PLACEMENT_3D('',#26572,#20876,#20877);
#17930=AXIS2_PLACEMENT_3D('',#26574,#20879,#20880);
#17931=AXIS2_PLACEMENT_3D('',#26585,#20884,#20885);
#17932=AXIS2_PLACEMENT_3D('',#26587,#20886,#20887);
#17933=AXIS2_PLACEMENT_3D('',#26600,#20888,#20889);
#17934=AXIS2_PLACEMENT_3D('',#26602,#20890,#20891);
#17935=AXIS2_PLACEMENT_3D('',#26604,#20893,#20894);
#17936=AXIS2_PLACEMENT_3D('',#26612,#20897,#20898);
#17937=AXIS2_PLACEMENT_3D('',#26627,#20902,#20903);
#17938=AXIS2_PLACEMENT_3D('',#26629,#20904,#20905);
#17939=AXIS2_PLACEMENT_3D('',#26642,#20906,#20907);
#17940=AXIS2_PLACEMENT_3D('',#26644,#20908,#20909);
#17941=AXIS2_PLACEMENT_3D('',#26646,#20911,#20912);
#17942=AXIS2_PLACEMENT_3D('',#26654,#20915,#20916);
#17943=AXIS2_PLACEMENT_3D('',#26669,#20920,#20921);
#17944=AXIS2_PLACEMENT_3D('',#26671,#20922,#20923);
#17945=AXIS2_PLACEMENT_3D('',#26684,#20924,#20925);
#17946=AXIS2_PLACEMENT_3D('',#26686,#20926,#20927);
#17947=AXIS2_PLACEMENT_3D('',#26688,#20929,#20930);
#17948=AXIS2_PLACEMENT_3D('',#26700,#20934,#20935);
#17949=AXIS2_PLACEMENT_3D('',#26705,#20936,#20937);
#17950=AXIS2_PLACEMENT_3D('',#26706,#20938,#20939);
#17951=AXIS2_PLACEMENT_3D('',#26707,#20940,#20941);
#17952=AXIS2_PLACEMENT_3D('',#26708,#20942,#20943);
#17953=AXIS2_PLACEMENT_3D('',#26709,#20944,#20945);
#17954=AXIS2_PLACEMENT_3D('',#26710,#20946,#20947);
#17955=AXIS2_PLACEMENT_3D('',#26711,#20948,#20949);
#17956=AXIS2_PLACEMENT_3D('',#26712,#20950,#20951);
#17957=AXIS2_PLACEMENT_3D('',#26713,#20952,#20953);
#17958=AXIS2_PLACEMENT_3D('',#26714,#20954,#20955);
#17959=AXIS2_PLACEMENT_3D('',#26715,#20956,#20957);
#17960=AXIS2_PLACEMENT_3D('',#26716,#20958,#20959);
#17961=AXIS2_PLACEMENT_3D('',#26717,#20960,#20961);
#17962=AXIS2_PLACEMENT_3D('',#26718,#20962,#20963);
#17963=AXIS2_PLACEMENT_3D('',#26719,#20964,#20965);
#17964=AXIS2_PLACEMENT_3D('',#26720,#20966,#20967);
#17965=AXIS2_PLACEMENT_3D('',#26721,#20968,#20969);
#17966=AXIS2_PLACEMENT_3D('',#26722,#20970,#20971);
#17967=AXIS2_PLACEMENT_3D('',#26723,#20972,#20973);
#17968=AXIS2_PLACEMENT_3D('',#26724,#20974,#20975);
#17969=AXIS2_PLACEMENT_3D('',#26725,#20976,#20977);
#17970=AXIS2_PLACEMENT_3D('',#26726,#20978,#20979);
#17971=AXIS2_PLACEMENT_3D('',#26730,#20982,#20983);
#17972=AXIS2_PLACEMENT_3D('',#26731,#20984,#20985);
#17973=AXIS2_PLACEMENT_3D('',#26732,#20986,#20987);
#17974=AXIS2_PLACEMENT_3D('',#26733,#20988,#20989);
#17975=AXIS2_PLACEMENT_3D('',#26734,#20990,#20991);
#17976=AXIS2_PLACEMENT_3D('',#26735,#20992,#20993);
#17977=AXIS2_PLACEMENT_3D('',#26736,#20994,#20995);
#17978=AXIS2_PLACEMENT_3D('',#26737,#20996,#20997);
#17979=AXIS2_PLACEMENT_3D('',#26738,#20998,#20999);
#17980=AXIS2_PLACEMENT_3D('',#26739,#21000,#21001);
#17981=AXIS2_PLACEMENT_3D('',#26740,#21002,#21003);
#17982=AXIS2_PLACEMENT_3D('',#26755,#21007,#21008);
#17983=AXIS2_PLACEMENT_3D('',#26757,#21009,#21010);
#17984=AXIS2_PLACEMENT_3D('',#26770,#21011,#21012);
#17985=AXIS2_PLACEMENT_3D('',#26772,#21013,#21014);
#17986=AXIS2_PLACEMENT_3D('',#26774,#21016,#21017);
#17987=AXIS2_PLACEMENT_3D('',#26782,#21020,#21021);
#17988=AXIS2_PLACEMENT_3D('',#26797,#21025,#21026);
#17989=AXIS2_PLACEMENT_3D('',#26799,#21027,#21028);
#17990=AXIS2_PLACEMENT_3D('',#26812,#21029,#21030);
#17991=AXIS2_PLACEMENT_3D('',#26814,#21031,#21032);
#17992=AXIS2_PLACEMENT_3D('',#26816,#21034,#21035);
#17993=AXIS2_PLACEMENT_3D('',#26824,#21038,#21039);
#17994=AXIS2_PLACEMENT_3D('',#26839,#21043,#21044);
#17995=AXIS2_PLACEMENT_3D('',#26841,#21045,#21046);
#17996=AXIS2_PLACEMENT_3D('',#26854,#21047,#21048);
#17997=AXIS2_PLACEMENT_3D('',#26856,#21049,#21050);
#17998=AXIS2_PLACEMENT_3D('',#26858,#21052,#21053);
#17999=AXIS2_PLACEMENT_3D('',#26866,#21056,#21057);
#18000=AXIS2_PLACEMENT_3D('',#26881,#21061,#21062);
#18001=AXIS2_PLACEMENT_3D('',#26883,#21063,#21064);
#18002=AXIS2_PLACEMENT_3D('',#26896,#21065,#21066);
#18003=AXIS2_PLACEMENT_3D('',#26898,#21067,#21068);
#18004=AXIS2_PLACEMENT_3D('',#26900,#21070,#21071);
#18005=AXIS2_PLACEMENT_3D('',#26908,#21074,#21075);
#18006=AXIS2_PLACEMENT_3D('',#26923,#21079,#21080);
#18007=AXIS2_PLACEMENT_3D('',#26925,#21081,#21082);
#18008=AXIS2_PLACEMENT_3D('',#26938,#21083,#21084);
#18009=AXIS2_PLACEMENT_3D('',#26940,#21085,#21086);
#18010=AXIS2_PLACEMENT_3D('',#26942,#21088,#21089);
#18011=AXIS2_PLACEMENT_3D('',#26950,#21092,#21093);
#18012=AXIS2_PLACEMENT_3D('',#26965,#21097,#21098);
#18013=AXIS2_PLACEMENT_3D('',#26967,#21099,#21100);
#18014=AXIS2_PLACEMENT_3D('',#26980,#21101,#21102);
#18015=AXIS2_PLACEMENT_3D('',#26982,#21103,#21104);
#18016=AXIS2_PLACEMENT_3D('',#26984,#21106,#21107);
#18017=AXIS2_PLACEMENT_3D('',#26992,#21110,#21111);
#18018=AXIS2_PLACEMENT_3D('',#27007,#21115,#21116);
#18019=AXIS2_PLACEMENT_3D('',#27009,#21117,#21118);
#18020=AXIS2_PLACEMENT_3D('',#27022,#21119,#21120);
#18021=AXIS2_PLACEMENT_3D('',#27024,#21121,#21122);
#18022=AXIS2_PLACEMENT_3D('',#27026,#21124,#21125);
#18023=AXIS2_PLACEMENT_3D('',#27037,#21129,#21130);
#18024=AXIS2_PLACEMENT_3D('',#27039,#21131,#21132);
#18025=AXIS2_PLACEMENT_3D('',#27042,#21134,#21135);
#18026=AXIS2_PLACEMENT_3D('',#27043,#21136,#21137);
#18027=AXIS2_PLACEMENT_3D('',#27051,#21138,#21139);
#18028=AXIS2_PLACEMENT_3D('',#27053,#21141,#21142);
#18029=AXIS2_PLACEMENT_3D('',#27064,#21146,#21147);
#18030=AXIS2_PLACEMENT_3D('',#27066,#21148,#21149);
#18031=AXIS2_PLACEMENT_3D('',#27079,#21150,#21151);
#18032=AXIS2_PLACEMENT_3D('',#27081,#21152,#21153);
#18033=AXIS2_PLACEMENT_3D('',#27083,#21155,#21156);
#18034=AXIS2_PLACEMENT_3D('',#27091,#21159,#21160);
#18035=AXIS2_PLACEMENT_3D('',#27106,#21164,#21165);
#18036=AXIS2_PLACEMENT_3D('',#27108,#21166,#21167);
#18037=AXIS2_PLACEMENT_3D('',#27121,#21168,#21169);
#18038=AXIS2_PLACEMENT_3D('',#27123,#21170,#21171);
#18039=AXIS2_PLACEMENT_3D('',#27125,#21173,#21174);
#18040=AXIS2_PLACEMENT_3D('',#27137,#21178,#21179);
#18041=AXIS2_PLACEMENT_3D('',#27142,#21180,#21181);
#18042=AXIS2_PLACEMENT_3D('',#27143,#21182,#21183);
#18043=AXIS2_PLACEMENT_3D('',#27144,#21184,#21185);
#18044=AXIS2_PLACEMENT_3D('',#27145,#21186,#21187);
#18045=AXIS2_PLACEMENT_3D('',#27146,#21188,#21189);
#18046=AXIS2_PLACEMENT_3D('',#27147,#21190,#21191);
#18047=AXIS2_PLACEMENT_3D('',#27148,#21192,#21193);
#18048=AXIS2_PLACEMENT_3D('',#27149,#21194,#21195);
#18049=AXIS2_PLACEMENT_3D('',#27150,#21196,#21197);
#18050=AXIS2_PLACEMENT_3D('',#27151,#21198,#21199);
#18051=AXIS2_PLACEMENT_3D('',#27152,#21200,#21201);
#18052=AXIS2_PLACEMENT_3D('',#27153,#21202,#21203);
#18053=AXIS2_PLACEMENT_3D('',#27154,#21204,#21205);
#18054=AXIS2_PLACEMENT_3D('',#27155,#21206,#21207);
#18055=AXIS2_PLACEMENT_3D('',#27156,#21208,#21209);
#18056=AXIS2_PLACEMENT_3D('',#27157,#21210,#21211);
#18057=AXIS2_PLACEMENT_3D('',#27158,#21212,#21213);
#18058=AXIS2_PLACEMENT_3D('',#27159,#21214,#21215);
#18059=AXIS2_PLACEMENT_3D('',#27160,#21216,#21217);
#18060=AXIS2_PLACEMENT_3D('',#27161,#21218,#21219);
#18061=AXIS2_PLACEMENT_3D('',#27162,#21220,#21221);
#18062=AXIS2_PLACEMENT_3D('',#27163,#21222,#21223);
#18063=AXIS2_PLACEMENT_3D('',#27164,#21224,#21225);
#18064=AXIS2_PLACEMENT_3D('',#27165,#21226,#21227);
#18065=AXIS2_PLACEMENT_3D('',#27166,#21228,#21229);
#18066=AXIS2_PLACEMENT_3D('',#27167,#21230,#21231);
#18067=AXIS2_PLACEMENT_3D('',#27168,#21232,#21233);
#18068=AXIS2_PLACEMENT_3D('',#27169,#21234,#21235);
#18069=AXIS2_PLACEMENT_3D('',#27173,#21238,#21239);
#18070=AXIS2_PLACEMENT_3D('',#27174,#21240,#21241);
#18071=AXIS2_PLACEMENT_3D('',#27175,#21242,#21243);
#18072=AXIS2_PLACEMENT_3D('',#27176,#21244,#21245);
#18073=AXIS2_PLACEMENT_3D('',#27177,#21246,#21247);
#18074=AXIS2_PLACEMENT_3D('',#27178,#21248,#21249);
#18075=AXIS2_PLACEMENT_3D('',#27179,#21250,#21251);
#18076=AXIS2_PLACEMENT_3D('',#27194,#21255,#21256);
#18077=AXIS2_PLACEMENT_3D('',#27196,#21257,#21258);
#18078=AXIS2_PLACEMENT_3D('',#27209,#21259,#21260);
#18079=AXIS2_PLACEMENT_3D('',#27211,#21261,#21262);
#18080=AXIS2_PLACEMENT_3D('',#27213,#21264,#21265);
#18081=AXIS2_PLACEMENT_3D('',#27221,#21268,#21269);
#18082=AXIS2_PLACEMENT_3D('',#27236,#21273,#21274);
#18083=AXIS2_PLACEMENT_3D('',#27238,#21275,#21276);
#18084=AXIS2_PLACEMENT_3D('',#27251,#21277,#21278);
#18085=AXIS2_PLACEMENT_3D('',#27253,#21279,#21280);
#18086=AXIS2_PLACEMENT_3D('',#27255,#21282,#21283);
#18087=AXIS2_PLACEMENT_3D('',#27263,#21286,#21287);
#18088=AXIS2_PLACEMENT_3D('',#27278,#21291,#21292);
#18089=AXIS2_PLACEMENT_3D('',#27280,#21293,#21294);
#18090=AXIS2_PLACEMENT_3D('',#27293,#21295,#21296);
#18091=AXIS2_PLACEMENT_3D('',#27295,#21297,#21298);
#18092=AXIS2_PLACEMENT_3D('',#27297,#21300,#21301);
#18093=AXIS2_PLACEMENT_3D('',#27305,#21304,#21305);
#18094=AXIS2_PLACEMENT_3D('',#27320,#21309,#21310);
#18095=AXIS2_PLACEMENT_3D('',#27322,#21311,#21312);
#18096=AXIS2_PLACEMENT_3D('',#27335,#21313,#21314);
#18097=AXIS2_PLACEMENT_3D('',#27337,#21315,#21316);
#18098=AXIS2_PLACEMENT_3D('',#27339,#21318,#21319);
#18099=AXIS2_PLACEMENT_3D('',#27347,#21322,#21323);
#18100=AXIS2_PLACEMENT_3D('',#27362,#21327,#21328);
#18101=AXIS2_PLACEMENT_3D('',#27364,#21329,#21330);
#18102=AXIS2_PLACEMENT_3D('',#27377,#21331,#21332);
#18103=AXIS2_PLACEMENT_3D('',#27379,#21333,#21334);
#18104=AXIS2_PLACEMENT_3D('',#27381,#21336,#21337);
#18105=AXIS2_PLACEMENT_3D('',#27389,#21340,#21341);
#18106=AXIS2_PLACEMENT_3D('',#27404,#21345,#21346);
#18107=AXIS2_PLACEMENT_3D('',#27406,#21347,#21348);
#18108=AXIS2_PLACEMENT_3D('',#27419,#21349,#21350);
#18109=AXIS2_PLACEMENT_3D('',#27421,#21351,#21352);
#18110=AXIS2_PLACEMENT_3D('',#27423,#21354,#21355);
#18111=AXIS2_PLACEMENT_3D('',#27431,#21358,#21359);
#18112=AXIS2_PLACEMENT_3D('',#27446,#21363,#21364);
#18113=AXIS2_PLACEMENT_3D('',#27448,#21365,#21366);
#18114=AXIS2_PLACEMENT_3D('',#27461,#21367,#21368);
#18115=AXIS2_PLACEMENT_3D('',#27463,#21369,#21370);
#18116=AXIS2_PLACEMENT_3D('',#27465,#21372,#21373);
#18117=AXIS2_PLACEMENT_3D('',#27473,#21376,#21377);
#18118=AXIS2_PLACEMENT_3D('',#27488,#21381,#21382);
#18119=AXIS2_PLACEMENT_3D('',#27490,#21383,#21384);
#18120=AXIS2_PLACEMENT_3D('',#27503,#21385,#21386);
#18121=AXIS2_PLACEMENT_3D('',#27505,#21387,#21388);
#18122=AXIS2_PLACEMENT_3D('',#27507,#21390,#21391);
#18123=AXIS2_PLACEMENT_3D('',#27518,#21395,#21396);
#18124=AXIS2_PLACEMENT_3D('',#27520,#21397,#21398);
#18125=AXIS2_PLACEMENT_3D('',#27523,#21400,#21401);
#18126=AXIS2_PLACEMENT_3D('',#27524,#21402,#21403);
#18127=AXIS2_PLACEMENT_3D('',#27532,#21404,#21405);
#18128=AXIS2_PLACEMENT_3D('',#27534,#21407,#21408);
#18129=AXIS2_PLACEMENT_3D('',#27545,#21412,#21413);
#18130=AXIS2_PLACEMENT_3D('',#27547,#21414,#21415);
#18131=AXIS2_PLACEMENT_3D('',#27560,#21416,#21417);
#18132=AXIS2_PLACEMENT_3D('',#27562,#21418,#21419);
#18133=AXIS2_PLACEMENT_3D('',#27564,#21421,#21422);
#18134=AXIS2_PLACEMENT_3D('',#27576,#21426,#21427);
#18135=AXIS2_PLACEMENT_3D('',#27581,#21428,#21429);
#18136=AXIS2_PLACEMENT_3D('',#27582,#21430,#21431);
#18137=AXIS2_PLACEMENT_3D('',#27583,#21432,#21433);
#18138=AXIS2_PLACEMENT_3D('',#27584,#21434,#21435);
#18139=AXIS2_PLACEMENT_3D('',#27585,#21436,#21437);
#18140=AXIS2_PLACEMENT_3D('',#27586,#21438,#21439);
#18141=AXIS2_PLACEMENT_3D('',#27587,#21440,#21441);
#18142=AXIS2_PLACEMENT_3D('',#27588,#21442,#21443);
#18143=AXIS2_PLACEMENT_3D('',#27589,#21444,#21445);
#18144=AXIS2_PLACEMENT_3D('',#27590,#21446,#21447);
#18145=AXIS2_PLACEMENT_3D('',#27591,#21448,#21449);
#18146=AXIS2_PLACEMENT_3D('',#27592,#21450,#21451);
#18147=AXIS2_PLACEMENT_3D('',#27593,#21452,#21453);
#18148=AXIS2_PLACEMENT_3D('',#27594,#21454,#21455);
#18149=AXIS2_PLACEMENT_3D('',#27595,#21456,#21457);
#18150=AXIS2_PLACEMENT_3D('',#27596,#21458,#21459);
#18151=AXIS2_PLACEMENT_3D('',#27597,#21460,#21461);
#18152=AXIS2_PLACEMENT_3D('',#27598,#21462,#21463);
#18153=AXIS2_PLACEMENT_3D('',#27599,#21464,#21465);
#18154=AXIS2_PLACEMENT_3D('',#27600,#21466,#21467);
#18155=AXIS2_PLACEMENT_3D('',#27601,#21468,#21469);
#18156=AXIS2_PLACEMENT_3D('',#27602,#21470,#21471);
#18157=AXIS2_PLACEMENT_3D('',#27603,#21472,#21473);
#18158=AXIS2_PLACEMENT_3D('',#27604,#21474,#21475);
#18159=AXIS2_PLACEMENT_3D('',#27605,#21476,#21477);
#18160=AXIS2_PLACEMENT_3D('',#27606,#21478,#21479);
#18161=AXIS2_PLACEMENT_3D('',#27607,#21480,#21481);
#18162=AXIS2_PLACEMENT_3D('',#27608,#21482,#21483);
#18163=AXIS2_PLACEMENT_3D('',#27609,#21484,#21485);
#18164=AXIS2_PLACEMENT_3D('',#27610,#21486,#21487);
#18165=AXIS2_PLACEMENT_3D('',#27611,#21488,#21489);
#18166=AXIS2_PLACEMENT_3D('',#27612,#21490,#21491);
#18167=AXIS2_PLACEMENT_3D('',#27616,#21494,#21495);
#18168=AXIS2_PLACEMENT_3D('',#27617,#21496,#21497);
#18169=AXIS2_PLACEMENT_3D('',#27618,#21498,#21499);
#18170=AXIS2_PLACEMENT_3D('',#27628,#21503,#21504);
#18171=AXIS2_PLACEMENT_3D('',#27630,#21505,#21506);
#18172=AXIS2_PLACEMENT_3D('',#27639,#21507,#21508);
#18173=AXIS2_PLACEMENT_3D('',#27641,#21509,#21510);
#18174=AXIS2_PLACEMENT_3D('',#27643,#21512,#21513);
#18175=AXIS2_PLACEMENT_3D('',#27651,#21516,#21517);
#18176=AXIS2_PLACEMENT_3D('',#27666,#21521,#21522);
#18177=AXIS2_PLACEMENT_3D('',#27668,#21523,#21524);
#18178=AXIS2_PLACEMENT_3D('',#27681,#21525,#21526);
#18179=AXIS2_PLACEMENT_3D('',#27683,#21527,#21528);
#18180=AXIS2_PLACEMENT_3D('',#27685,#21530,#21531);
#18181=AXIS2_PLACEMENT_3D('',#27693,#21534,#21535);
#18182=AXIS2_PLACEMENT_3D('',#27708,#21539,#21540);
#18183=AXIS2_PLACEMENT_3D('',#27710,#21541,#21542);
#18184=AXIS2_PLACEMENT_3D('',#27723,#21543,#21544);
#18185=AXIS2_PLACEMENT_3D('',#27725,#21545,#21546);
#18186=AXIS2_PLACEMENT_3D('',#27727,#21548,#21549);
#18187=AXIS2_PLACEMENT_3D('',#27735,#21552,#21553);
#18188=AXIS2_PLACEMENT_3D('',#27750,#21557,#21558);
#18189=AXIS2_PLACEMENT_3D('',#27752,#21559,#21560);
#18190=AXIS2_PLACEMENT_3D('',#27765,#21561,#21562);
#18191=AXIS2_PLACEMENT_3D('',#27767,#21563,#21564);
#18192=AXIS2_PLACEMENT_3D('',#27769,#21566,#21567);
#18193=AXIS2_PLACEMENT_3D('',#27777,#21570,#21571);
#18194=AXIS2_PLACEMENT_3D('',#27792,#21575,#21576);
#18195=AXIS2_PLACEMENT_3D('',#27794,#21577,#21578);
#18196=AXIS2_PLACEMENT_3D('',#27807,#21579,#21580);
#18197=AXIS2_PLACEMENT_3D('',#27809,#21581,#21582);
#18198=AXIS2_PLACEMENT_3D('',#27811,#21584,#21585);
#18199=AXIS2_PLACEMENT_3D('',#27819,#21588,#21589);
#18200=AXIS2_PLACEMENT_3D('',#27834,#21593,#21594);
#18201=AXIS2_PLACEMENT_3D('',#27836,#21595,#21596);
#18202=AXIS2_PLACEMENT_3D('',#27849,#21597,#21598);
#18203=AXIS2_PLACEMENT_3D('',#27851,#21599,#21600);
#18204=AXIS2_PLACEMENT_3D('',#27853,#21602,#21603);
#18205=AXIS2_PLACEMENT_3D('',#27861,#21606,#21607);
#18206=AXIS2_PLACEMENT_3D('',#27876,#21611,#21612);
#18207=AXIS2_PLACEMENT_3D('',#27878,#21613,#21614);
#18208=AXIS2_PLACEMENT_3D('',#27891,#21615,#21616);
#18209=AXIS2_PLACEMENT_3D('',#27893,#21617,#21618);
#18210=AXIS2_PLACEMENT_3D('',#27895,#21620,#21621);
#18211=AXIS2_PLACEMENT_3D('',#27903,#21624,#21625);
#18212=AXIS2_PLACEMENT_3D('',#27918,#21629,#21630);
#18213=AXIS2_PLACEMENT_3D('',#27920,#21631,#21632);
#18214=AXIS2_PLACEMENT_3D('',#27933,#21633,#21634);
#18215=AXIS2_PLACEMENT_3D('',#27935,#21635,#21636);
#18216=AXIS2_PLACEMENT_3D('',#27937,#21638,#21639);
#18217=AXIS2_PLACEMENT_3D('',#27945,#21642,#21643);
#18218=AXIS2_PLACEMENT_3D('',#27960,#21647,#21648);
#18219=AXIS2_PLACEMENT_3D('',#27962,#21649,#21650);
#18220=AXIS2_PLACEMENT_3D('',#27975,#21651,#21652);
#18221=AXIS2_PLACEMENT_3D('',#27977,#21653,#21654);
#18222=AXIS2_PLACEMENT_3D('',#27979,#21656,#21657);
#18223=AXIS2_PLACEMENT_3D('',#27987,#21660,#21661);
#18224=AXIS2_PLACEMENT_3D('',#27989,#21662,#21663);
#18225=AXIS2_PLACEMENT_3D('',#27992,#21665,#21666);
#18226=AXIS2_PLACEMENT_3D('',#27993,#21667,#21668);
#18227=AXIS2_PLACEMENT_3D('',#27997,#21669,#21670);
#18228=AXIS2_PLACEMENT_3D('',#27999,#21672,#21673);
#18229=AXIS2_PLACEMENT_3D('',#28000,#21674,#21675);
#18230=AXIS2_PLACEMENT_3D('',#28001,#21676,#21677);
#18231=AXIS2_PLACEMENT_3D('',#28002,#21678,#21679);
#18232=AXIS2_PLACEMENT_3D('',#28003,#21680,#21681);
#18233=AXIS2_PLACEMENT_3D('',#28004,#21682,#21683);
#18234=AXIS2_PLACEMENT_3D('',#28005,#21684,#21685);
#18235=AXIS2_PLACEMENT_3D('',#28006,#21686,#21687);
#18236=AXIS2_PLACEMENT_3D('',#28007,#21688,#21689);
#18237=AXIS2_PLACEMENT_3D('',#28008,#21690,#21691);
#18238=AXIS2_PLACEMENT_3D('',#28009,#21692,#21693);
#18239=AXIS2_PLACEMENT_3D('',#28010,#21694,#21695);
#18240=AXIS2_PLACEMENT_3D('',#28011,#21696,#21697);
#18241=AXIS2_PLACEMENT_3D('',#28012,#21698,#21699);
#18242=AXIS2_PLACEMENT_3D('',#28013,#21700,#21701);
#18243=AXIS2_PLACEMENT_3D('',#28014,#21702,#21703);
#18244=AXIS2_PLACEMENT_3D('',#28015,#21704,#21705);
#18245=AXIS2_PLACEMENT_3D('',#28016,#21706,#21707);
#18246=AXIS2_PLACEMENT_3D('',#28017,#21708,#21709);
#18247=AXIS2_PLACEMENT_3D('',#28018,#21710,#21711);
#18248=AXIS2_PLACEMENT_3D('',#28019,#21712,#21713);
#18249=AXIS2_PLACEMENT_3D('',#28020,#21714,#21715);
#18250=AXIS2_PLACEMENT_3D('',#28021,#21716,#21717);
#18251=AXIS2_PLACEMENT_3D('',#28022,#21718,#21719);
#18252=AXIS2_PLACEMENT_3D('',#28023,#21720,#21721);
#18253=AXIS2_PLACEMENT_3D('',#28024,#21722,#21723);
#18254=AXIS2_PLACEMENT_3D('',#28025,#21724,#21725);
#18255=AXIS2_PLACEMENT_3D('',#28026,#21726,#21727);
#18256=AXIS2_PLACEMENT_3D('',#28027,#21728,#21729);
#18257=AXIS2_PLACEMENT_3D('',#28028,#21730,#21731);
#18258=AXIS2_PLACEMENT_3D('',#28029,#21732,#21733);
#18259=AXIS2_PLACEMENT_3D('',#28030,#21734,#21735);
#18260=AXIS2_PLACEMENT_3D('',#28031,#21736,#21737);
#18261=AXIS2_PLACEMENT_3D('',#28033,#21738,#21739);
#18262=AXIS2_PLACEMENT_3D('',#28035,#21741,#21742);
#18263=AXIS2_PLACEMENT_3D('',#28037,#21743,#21744);
#18264=AXIS2_PLACEMENT_3D('',#28039,#21746,#21747);
#18265=AXIS2_PLACEMENT_3D('',#28043,#21750,#21751);
#18266=AXIS2_PLACEMENT_3D('',#28044,#21752,#21753);
#18267=AXIS2_PLACEMENT_3D('',#28045,#21754,#21755);
#18268=AXIS2_PLACEMENT_3D('',#28046,#21756,#21757);
#18269=AXIS2_PLACEMENT_3D('',#28047,#21758,#21759);
#18270=AXIS2_PLACEMENT_3D('',#28048,#21760,#21761);
#18271=AXIS2_PLACEMENT_3D('',#28049,#21762,#21763);
#18272=AXIS2_PLACEMENT_3D('',#28050,#21764,#21765);
#18273=AXIS2_PLACEMENT_3D('',#28051,#21766,#21767);
#18274=AXIS2_PLACEMENT_3D('',#28052,#21768,#21769);
#18275=AXIS2_PLACEMENT_3D('',#28053,#21770,#21771);
#18276=AXIS2_PLACEMENT_3D('',#28054,#21772,#21773);
#18277=AXIS2_PLACEMENT_3D('',#28055,#21774,#21775);
#18278=AXIS2_PLACEMENT_3D('',#28056,#21776,#21777);
#18279=AXIS2_PLACEMENT_3D('',#28057,#21778,#21779);
#18280=AXIS2_PLACEMENT_3D('',#28058,#21780,#21781);
#18281=AXIS2_PLACEMENT_3D('',#28059,#21782,#21783);
#18282=AXIS2_PLACEMENT_3D('',#28060,#21784,#21785);
#18283=AXIS2_PLACEMENT_3D('',#28061,#21786,#21787);
#18284=AXIS2_PLACEMENT_3D('',#28062,#21788,#21789);
#18285=AXIS2_PLACEMENT_3D('',#28063,#21790,#21791);
#18286=AXIS2_PLACEMENT_3D('',#28064,#21792,#21793);
#18287=AXIS2_PLACEMENT_3D('',#28065,#21794,#21795);
#18288=AXIS2_PLACEMENT_3D('',#28066,#21796,#21797);
#18289=AXIS2_PLACEMENT_3D('',#28067,#21798,#21799);
#18290=AXIS2_PLACEMENT_3D('',#28068,#21800,#21801);
#18291=AXIS2_PLACEMENT_3D('',#28069,#21802,#21803);
#18292=AXIS2_PLACEMENT_3D('',#28070,#21804,#21805);
#18293=AXIS2_PLACEMENT_3D('',#28071,#21806,#21807);
#18294=AXIS2_PLACEMENT_3D('',#28072,#21808,#21809);
#18295=AXIS2_PLACEMENT_3D('',#28073,#21810,#21811);
#18296=AXIS2_PLACEMENT_3D('',#28074,#21812,#21813);
#18297=AXIS2_PLACEMENT_3D('',#28075,#21814,#21815);
#18298=AXIS2_PLACEMENT_3D('',#28076,#21816,#21817);
#18299=AXIS2_PLACEMENT_3D('',#28077,#21818,#21819);
#18300=AXIS2_PLACEMENT_3D('',#28083,#21823,#21824);
#18301=AXIS2_PLACEMENT_3D('',#28084,#21825,#21826);
#18302=AXIS2_PLACEMENT_3D('',#28085,#21827,#21828);
#18303=AXIS2_PLACEMENT_3D('',#28094,#21831,#21832);
#18304=AXIS2_PLACEMENT_3D('',#28096,#21833,#21834);
#18305=AXIS2_PLACEMENT_3D('',#28106,#21835,#21836);
#18306=AXIS2_PLACEMENT_3D('',#28112,#21840,#21841);
#18307=AXIS2_PLACEMENT_3D('',#28114,#21842,#21843);
#18308=AXIS2_PLACEMENT_3D('',#28121,#21845,#21846);
#18309=AXIS2_PLACEMENT_3D('',#28133,#21850,#21851);
#18310=AXIS2_PLACEMENT_3D('',#28135,#21852,#21853);
#18311=AXIS2_PLACEMENT_3D('',#28144,#21854,#21855);
#18312=AXIS2_PLACEMENT_3D('',#28148,#21858,#21859);
#18313=AXIS2_PLACEMENT_3D('',#28156,#21861,#21862);
#18314=AXIS2_PLACEMENT_3D('',#28157,#21863,#21864);
#18315=AXIS2_PLACEMENT_3D('',#28166,#21867,#21868);
#18316=AXIS2_PLACEMENT_3D('',#28168,#21869,#21870);
#18317=AXIS2_PLACEMENT_3D('',#28178,#21871,#21872);
#18318=AXIS2_PLACEMENT_3D('',#28184,#21876,#21877);
#18319=AXIS2_PLACEMENT_3D('',#28186,#21878,#21879);
#18320=AXIS2_PLACEMENT_3D('',#28193,#21881,#21882);
#18321=AXIS2_PLACEMENT_3D('',#28205,#21886,#21887);
#18322=AXIS2_PLACEMENT_3D('',#28207,#21888,#21889);
#18323=AXIS2_PLACEMENT_3D('',#28216,#21890,#21891);
#18324=AXIS2_PLACEMENT_3D('',#28220,#21894,#21895);
#18325=AXIS2_PLACEMENT_3D('',#28228,#21897,#21898);
#18326=AXIS2_PLACEMENT_3D('',#28229,#21899,#21900);
#18327=AXIS2_PLACEMENT_3D('',#28238,#21903,#21904);
#18328=AXIS2_PLACEMENT_3D('',#28240,#21905,#21906);
#18329=AXIS2_PLACEMENT_3D('',#28250,#21907,#21908);
#18330=AXIS2_PLACEMENT_3D('',#28256,#21912,#21913);
#18331=AXIS2_PLACEMENT_3D('',#28258,#21914,#21915);
#18332=AXIS2_PLACEMENT_3D('',#28265,#21917,#21918);
#18333=AXIS2_PLACEMENT_3D('',#28274,#21921,#21922);
#18334=AXIS2_PLACEMENT_3D('',#28276,#21923,#21924);
#18335=AXIS2_PLACEMENT_3D('',#28281,#21925,#21926);
#18336=AXIS2_PLACEMENT_3D('',#28285,#21929,#21930);
#18337=AXIS2_PLACEMENT_3D('',#28287,#21931,#21932);
#18338=AXIS2_PLACEMENT_3D('',#28290,#21934,#21935);
#18339=AXIS2_PLACEMENT_3D('',#28291,#21936,#21937);
#18340=AXIS2_PLACEMENT_3D('',#28293,#21938,#21939);
#18341=AXIS2_PLACEMENT_3D('',#28294,#21940,#21941);
#18342=AXIS2_PLACEMENT_3D('',#28297,#21943,#21944);
#18343=AXIS2_PLACEMENT_3D('',#28298,#21945,#21946);
#18344=AXIS2_PLACEMENT_3D('',#28299,#21947,#21948);
#18345=AXIS2_PLACEMENT_3D('',#28300,#21949,#21950);
#18346=AXIS2_PLACEMENT_3D('',#28301,#21951,#21952);
#18347=AXIS2_PLACEMENT_3D('',#28302,#21953,#21954);
#18348=AXIS2_PLACEMENT_3D('',#28303,#21955,#21956);
#18349=AXIS2_PLACEMENT_3D('',#28304,#21957,#21958);
#18350=AXIS2_PLACEMENT_3D('',#28305,#21959,#21960);
#18351=AXIS2_PLACEMENT_3D('',#28306,#21961,#21962);
#18352=AXIS2_PLACEMENT_3D('',#28307,#21963,#21964);
#18353=AXIS2_PLACEMENT_3D('',#28308,#21965,#21966);
#18354=AXIS2_PLACEMENT_3D('',#28309,#21967,#21968);
#18355=AXIS2_PLACEMENT_3D('',#28310,#21969,#21970);
#18356=AXIS2_PLACEMENT_3D('',#28311,#21971,#21972);
#18357=AXIS2_PLACEMENT_3D('',#28312,#21973,#21974);
#18358=AXIS2_PLACEMENT_3D('',#28313,#21975,#21976);
#18359=AXIS2_PLACEMENT_3D('',#28314,#21977,#21978);
#18360=AXIS2_PLACEMENT_3D('',#28315,#21979,#21980);
#18361=AXIS2_PLACEMENT_3D('',#28316,#21981,#21982);
#18362=AXIS2_PLACEMENT_3D('',#28317,#21983,#21984);
#18363=AXIS2_PLACEMENT_3D('',#28318,#21985,#21986);
#18364=AXIS2_PLACEMENT_3D('',#28319,#21987,#21988);
#18365=AXIS2_PLACEMENT_3D('',#28320,#21989,#21990);
#18366=AXIS2_PLACEMENT_3D('',#28321,#21991,#21992);
#18367=AXIS2_PLACEMENT_3D('',#28322,#21993,#21994);
#18368=AXIS2_PLACEMENT_3D('',#28323,#21995,#21996);
#18369=AXIS2_PLACEMENT_3D('',#28324,#21997,#21998);
#18370=AXIS2_PLACEMENT_3D('',#28325,#21999,#22000);
#18371=AXIS2_PLACEMENT_3D('',#28326,#22001,#22002);
#18372=AXIS2_PLACEMENT_3D('',#28327,#22003,#22004);
#18373=AXIS2_PLACEMENT_3D('',#28328,#22005,#22006);
#18374=AXIS2_PLACEMENT_3D('',#28329,#22007,#22008);
#18375=AXIS2_PLACEMENT_3D('',#28330,#22009,#22010);
#18376=AXIS2_PLACEMENT_3D('',#28331,#22011,#22012);
#18377=AXIS2_PLACEMENT_3D('',#28332,#22013,#22014);
#18378=AXIS2_PLACEMENT_3D('',#28333,#22015,#22016);
#18379=AXIS2_PLACEMENT_3D('',#28334,#22017,#22018);
#18380=AXIS2_PLACEMENT_3D('',#28335,#22019,#22020);
#18381=AXIS2_PLACEMENT_3D('',#28336,#22021,#22022);
#18382=AXIS2_PLACEMENT_3D('',#28337,#22023,#22024);
#18383=AXIS2_PLACEMENT_3D('',#28338,#22025,#22026);
#18384=AXIS2_PLACEMENT_3D('',#28339,#22027,#22028);
#18385=AXIS2_PLACEMENT_3D('',#28340,#22029,#22030);
#18386=AXIS2_PLACEMENT_3D('',#28341,#22031,#22032);
#18387=AXIS2_PLACEMENT_3D('',#28342,#22033,#22034);
#18388=AXIS2_PLACEMENT_3D('',#28343,#22035,#22036);
#18389=AXIS2_PLACEMENT_3D('',#28344,#22037,#22038);
#18390=AXIS2_PLACEMENT_3D('',#28345,#22039,#22040);
#18391=AXIS2_PLACEMENT_3D('',#28346,#22041,#22042);
#18392=AXIS2_PLACEMENT_3D('',#28347,#22043,#22044);
#18393=AXIS2_PLACEMENT_3D('',#28348,#22045,#22046);
#18394=AXIS2_PLACEMENT_3D('',#28349,#22047,#22048);
#18395=AXIS2_PLACEMENT_3D('',#28350,#22049,#22050);
#18396=AXIS2_PLACEMENT_3D('',#28351,#22051,#22052);
#18397=AXIS2_PLACEMENT_3D('',#28352,#22053,#22054);
#18398=AXIS2_PLACEMENT_3D('',#28353,#22055,#22056);
#18399=AXIS2_PLACEMENT_3D('',#28354,#22057,#22058);
#18400=AXIS2_PLACEMENT_3D('',#28355,#22059,#22060);
#18401=AXIS2_PLACEMENT_3D('',#28356,#22061,#22062);
#18402=AXIS2_PLACEMENT_3D('',#28357,#22063,#22064);
#18403=AXIS2_PLACEMENT_3D('',#28358,#22065,#22066);
#18404=AXIS2_PLACEMENT_3D('',#28359,#22067,#22068);
#18405=AXIS2_PLACEMENT_3D('',#28360,#22069,#22070);
#18406=AXIS2_PLACEMENT_3D('',#28361,#22071,#22072);
#18407=AXIS2_PLACEMENT_3D('',#28362,#22073,#22074);
#18408=AXIS2_PLACEMENT_3D('',#28363,#22075,#22076);
#18409=AXIS2_PLACEMENT_3D('',#28364,#22077,#22078);
#18410=AXIS2_PLACEMENT_3D('',#28365,#22079,#22080);
#18411=AXIS2_PLACEMENT_3D('',#28366,#22081,#22082);
#18412=AXIS2_PLACEMENT_3D('',#28367,#22083,#22084);
#18413=AXIS2_PLACEMENT_3D('',#28368,#22085,#22086);
#18414=AXIS2_PLACEMENT_3D('',#28369,#22087,#22088);
#18415=AXIS2_PLACEMENT_3D('',#28370,#22089,#22090);
#18416=AXIS2_PLACEMENT_3D('',#28371,#22091,#22092);
#18417=AXIS2_PLACEMENT_3D('',#28372,#22093,#22094);
#18418=AXIS2_PLACEMENT_3D('',#28373,#22095,#22096);
#18419=AXIS2_PLACEMENT_3D('',#28374,#22097,#22098);
#18420=AXIS2_PLACEMENT_3D('',#28375,#22099,#22100);
#18421=AXIS2_PLACEMENT_3D('',#28376,#22101,#22102);
#18422=AXIS2_PLACEMENT_3D('',#28377,#22103,#22104);
#18423=AXIS2_PLACEMENT_3D('',#28378,#22105,#22106);
#18424=AXIS2_PLACEMENT_3D('',#28379,#22107,#22108);
#18425=AXIS2_PLACEMENT_3D('',#28380,#22109,#22110);
#18426=AXIS2_PLACEMENT_3D('',#28381,#22111,#22112);
#18427=AXIS2_PLACEMENT_3D('',#28382,#22113,#22114);
#18428=AXIS2_PLACEMENT_3D('',#28383,#22115,#22116);
#18429=AXIS2_PLACEMENT_3D('',#28384,#22117,#22118);
#18430=AXIS2_PLACEMENT_3D('',#28385,#22119,#22120);
#18431=AXIS2_PLACEMENT_3D('',#28386,#22121,#22122);
#18432=AXIS2_PLACEMENT_3D('',#28387,#22123,#22124);
#18433=AXIS2_PLACEMENT_3D('',#28388,#22125,#22126);
#18434=AXIS2_PLACEMENT_3D('',#28389,#22127,#22128);
#18435=AXIS2_PLACEMENT_3D('',#28390,#22129,#22130);
#18436=AXIS2_PLACEMENT_3D('',#28391,#22131,#22132);
#18437=AXIS2_PLACEMENT_3D('',#28392,#22133,#22134);
#18438=AXIS2_PLACEMENT_3D('',#28393,#22135,#22136);
#18439=AXIS2_PLACEMENT_3D('',#28394,#22137,#22138);
#18440=AXIS2_PLACEMENT_3D('',#28395,#22139,#22140);
#18441=AXIS2_PLACEMENT_3D('',#28396,#22141,#22142);
#18442=AXIS2_PLACEMENT_3D('',#28397,#22143,#22144);
#18443=AXIS2_PLACEMENT_3D('',#28398,#22145,#22146);
#18444=AXIS2_PLACEMENT_3D('',#28400,#22147,#22148);
#18445=AXIS2_PLACEMENT_3D('',#28403,#22150,#22151);
#18446=AXIS2_PLACEMENT_3D('',#28404,#22152,#22153);
#18447=AXIS2_PLACEMENT_3D('',#28406,#22154,#22155);
#18448=AXIS2_PLACEMENT_3D('',#28408,#22156,#22157);
#18449=AXIS2_PLACEMENT_3D('',#28410,#22158,#22159);
#18450=AXIS2_PLACEMENT_3D('',#28412,#22160,#22161);
#18451=AXIS2_PLACEMENT_3D('',#28414,#22162,#22163);
#18452=AXIS2_PLACEMENT_3D('',#28416,#22164,#22165);
#18453=AXIS2_PLACEMENT_3D('',#28417,#22166,#22167);
#18454=AXIS2_PLACEMENT_3D('',#28420,#22169,#22170);
#18455=AXIS2_PLACEMENT_3D('',#28421,#22171,#22172);
#18456=AXIS2_PLACEMENT_3D('',#28424,#22174,#22175);
#18457=AXIS2_PLACEMENT_3D('',#28425,#22176,#22177);
#18458=AXIS2_PLACEMENT_3D('',#28428,#22179,#22180);
#18459=AXIS2_PLACEMENT_3D('',#28429,#22181,#22182);
#18460=AXIS2_PLACEMENT_3D('',#28432,#22184,#22185);
#18461=AXIS2_PLACEMENT_3D('',#28433,#22186,#22187);
#18462=AXIS2_PLACEMENT_3D('',#28436,#22189,#22190);
#18463=AXIS2_PLACEMENT_3D('',#28437,#22191,#22192);
#18464=AXIS2_PLACEMENT_3D('',#28440,#22194,#22195);
#18465=AXIS2_PLACEMENT_3D('',#28441,#22196,#22197);
#18466=AXIS2_PLACEMENT_3D('',#28444,#22199,#22200);
#18467=AXIS2_PLACEMENT_3D('',#28445,#22201,#22202);
#18468=AXIS2_PLACEMENT_3D('',#28448,#22204,#22205);
#18469=AXIS2_PLACEMENT_3D('',#28449,#22206,#22207);
#18470=AXIS2_PLACEMENT_3D('',#28452,#22209,#22210);
#18471=AXIS2_PLACEMENT_3D('',#28453,#22211,#22212);
#18472=AXIS2_PLACEMENT_3D('',#28456,#22214,#22215);
#18473=AXIS2_PLACEMENT_3D('',#28457,#22216,#22217);
#18474=AXIS2_PLACEMENT_3D('',#28459,#22219,#22220);
#18475=AXIS2_PLACEMENT_3D('',#28460,#22221,#22222);
#18476=AXIS2_PLACEMENT_3D('',#28461,#22223,#22224);
#18477=AXIS2_PLACEMENT_3D('',#28462,#22225,#22226);
#18478=AXIS2_PLACEMENT_3D('',#28463,#22227,#22228);
#18479=AXIS2_PLACEMENT_3D('',#28464,#22229,#22230);
#18480=AXIS2_PLACEMENT_3D('',#28465,#22231,#22232);
#18481=AXIS2_PLACEMENT_3D('',#28466,#22233,#22234);
#18482=AXIS2_PLACEMENT_3D('',#28467,#22235,#22236);
#18483=AXIS2_PLACEMENT_3D('',#28468,#22237,#22238);
#18484=AXIS2_PLACEMENT_3D('',#28469,#22239,#22240);
#18485=AXIS2_PLACEMENT_3D('',#28470,#22241,#22242);
#18486=AXIS2_PLACEMENT_3D('',#28471,#22243,#22244);
#18487=AXIS2_PLACEMENT_3D('',#28472,#22245,#22246);
#18488=AXIS2_PLACEMENT_3D('',#28473,#22247,#22248);
#18489=AXIS2_PLACEMENT_3D('',#28474,#22249,#22250);
#18490=AXIS2_PLACEMENT_3D('',#28475,#22251,#22252);
#18491=AXIS2_PLACEMENT_3D('',#28476,#22253,#22254);
#18492=AXIS2_PLACEMENT_3D('',#28477,#22255,#22256);
#18493=AXIS2_PLACEMENT_3D('',#28478,#22257,#22258);
#18494=AXIS2_PLACEMENT_3D('',#28479,#22259,#22260);
#18495=AXIS2_PLACEMENT_3D('',#28480,#22261,#22262);
#18496=AXIS2_PLACEMENT_3D('',#28481,#22263,#22264);
#18497=AXIS2_PLACEMENT_3D('',#28482,#22265,#22266);
#18498=AXIS2_PLACEMENT_3D('',#28483,#22267,#22268);
#18499=AXIS2_PLACEMENT_3D('',#28484,#22269,#22270);
#18500=AXIS2_PLACEMENT_3D('',#28485,#22271,#22272);
#18501=AXIS2_PLACEMENT_3D('',#28486,#22273,#22274);
#18502=AXIS2_PLACEMENT_3D('',#28487,#22275,#22276);
#18503=AXIS2_PLACEMENT_3D('',#28488,#22277,#22278);
#18504=AXIS2_PLACEMENT_3D('',#28489,#22279,#22280);
#18505=AXIS2_PLACEMENT_3D('',#28490,#22281,#22282);
#18506=AXIS2_PLACEMENT_3D('',#28491,#22283,#22284);
#18507=AXIS2_PLACEMENT_3D('',#28492,#22285,#22286);
#18508=AXIS2_PLACEMENT_3D('',#28493,#22287,#22288);
#18509=AXIS2_PLACEMENT_3D('',#28494,#22289,#22290);
#18510=AXIS2_PLACEMENT_3D('',#28495,#22291,#22292);
#18511=AXIS2_PLACEMENT_3D('',#28496,#22293,#22294);
#18512=AXIS2_PLACEMENT_3D('',#28497,#22295,#22296);
#18513=AXIS2_PLACEMENT_3D('',#28498,#22297,#22298);
#18514=AXIS2_PLACEMENT_3D('',#28499,#22299,#22300);
#18515=AXIS2_PLACEMENT_3D('',#28500,#22301,#22302);
#18516=AXIS2_PLACEMENT_3D('',#28501,#22303,#22304);
#18517=AXIS2_PLACEMENT_3D('',#28502,#22305,#22306);
#18518=AXIS2_PLACEMENT_3D('',#28503,#22307,#22308);
#18519=AXIS2_PLACEMENT_3D('',#28504,#22309,#22310);
#18520=AXIS2_PLACEMENT_3D('',#28505,#22311,#22312);
#18521=AXIS2_PLACEMENT_3D('',#28506,#22313,#22314);
#18522=AXIS2_PLACEMENT_3D('',#28507,#22315,#22316);
#18523=AXIS2_PLACEMENT_3D('',#28508,#22317,#22318);
#18524=AXIS2_PLACEMENT_3D('',#28509,#22319,#22320);
#18525=AXIS2_PLACEMENT_3D('',#28510,#22321,#22322);
#18526=AXIS2_PLACEMENT_3D('',#28511,#22323,#22324);
#18527=AXIS2_PLACEMENT_3D('',#28512,#22325,#22326);
#18528=AXIS2_PLACEMENT_3D('',#28513,#22327,#22328);
#18529=AXIS2_PLACEMENT_3D('',#28514,#22329,#22330);
#18530=AXIS2_PLACEMENT_3D('',#28515,#22331,#22332);
#18531=AXIS2_PLACEMENT_3D('',#28516,#22333,#22334);
#18532=AXIS2_PLACEMENT_3D('',#28517,#22335,#22336);
#18533=AXIS2_PLACEMENT_3D('',#28518,#22337,#22338);
#18534=AXIS2_PLACEMENT_3D('',#28519,#22339,#22340);
#18535=AXIS2_PLACEMENT_3D('',#28520,#22341,#22342);
#18536=AXIS2_PLACEMENT_3D('',#28521,#22343,#22344);
#18537=AXIS2_PLACEMENT_3D('',#28522,#22345,#22346);
#18538=AXIS2_PLACEMENT_3D('',#28523,#22347,#22348);
#18539=AXIS2_PLACEMENT_3D('',#28524,#22349,#22350);
#18540=AXIS2_PLACEMENT_3D('',#28525,#22351,#22352);
#18541=AXIS2_PLACEMENT_3D('',#28526,#22353,#22354);
#18542=AXIS2_PLACEMENT_3D('',#28527,#22355,#22356);
#18543=AXIS2_PLACEMENT_3D('',#28528,#22357,#22358);
#18544=AXIS2_PLACEMENT_3D('',#28529,#22359,#22360);
#18545=AXIS2_PLACEMENT_3D('',#28530,#22361,#22362);
#18546=AXIS2_PLACEMENT_3D('',#28531,#22363,#22364);
#18547=AXIS2_PLACEMENT_3D('',#28532,#22365,#22366);
#18548=AXIS2_PLACEMENT_3D('',#28533,#22367,#22368);
#18549=AXIS2_PLACEMENT_3D('',#28534,#22369,#22370);
#18550=AXIS2_PLACEMENT_3D('',#28535,#22371,#22372);
#18551=AXIS2_PLACEMENT_3D('',#28536,#22373,#22374);
#18552=AXIS2_PLACEMENT_3D('',#28537,#22375,#22376);
#18553=AXIS2_PLACEMENT_3D('',#28538,#22377,#22378);
#18554=AXIS2_PLACEMENT_3D('',#28539,#22379,#22380);
#18555=AXIS2_PLACEMENT_3D('',#28540,#22381,#22382);
#18556=AXIS2_PLACEMENT_3D('',#28541,#22383,#22384);
#18557=AXIS2_PLACEMENT_3D('',#28542,#22385,#22386);
#18558=AXIS2_PLACEMENT_3D('',#28543,#22387,#22388);
#18559=AXIS2_PLACEMENT_3D('',#28544,#22389,#22390);
#18560=AXIS2_PLACEMENT_3D('',#28545,#22391,#22392);
#18561=AXIS2_PLACEMENT_3D('',#28546,#22393,#22394);
#18562=AXIS2_PLACEMENT_3D('',#28547,#22395,#22396);
#18563=AXIS2_PLACEMENT_3D('',#28548,#22397,#22398);
#18564=AXIS2_PLACEMENT_3D('',#28549,#22399,#22400);
#18565=AXIS2_PLACEMENT_3D('',#28550,#22401,#22402);
#18566=AXIS2_PLACEMENT_3D('',#28551,#22403,#22404);
#18567=AXIS2_PLACEMENT_3D('',#28552,#22405,#22406);
#18568=AXIS2_PLACEMENT_3D('',#28553,#22407,#22408);
#18569=AXIS2_PLACEMENT_3D('',#28554,#22409,#22410);
#18570=AXIS2_PLACEMENT_3D('',#28555,#22411,#22412);
#18571=AXIS2_PLACEMENT_3D('',#28556,#22413,#22414);
#18572=AXIS2_PLACEMENT_3D('',#28557,#22415,#22416);
#18573=AXIS2_PLACEMENT_3D('',#28558,#22417,#22418);
#18574=AXIS2_PLACEMENT_3D('',#28559,#22419,#22420);
#18575=AXIS2_PLACEMENT_3D('',#28560,#22421,#22422);
#18576=AXIS2_PLACEMENT_3D('',#28561,#22423,#22424);
#18577=AXIS2_PLACEMENT_3D('',#28562,#22425,#22426);
#18578=AXIS2_PLACEMENT_3D('',#28563,#22427,#22428);
#18579=AXIS2_PLACEMENT_3D('',#28564,#22429,#22430);
#18580=AXIS2_PLACEMENT_3D('',#28565,#22431,#22432);
#18581=AXIS2_PLACEMENT_3D('',#28566,#22433,#22434);
#18582=AXIS2_PLACEMENT_3D('',#28567,#22435,#22436);
#18583=AXIS2_PLACEMENT_3D('',#28568,#22437,#22438);
#18584=AXIS2_PLACEMENT_3D('',#28569,#22439,#22440);
#18585=AXIS2_PLACEMENT_3D('',#28570,#22441,#22442);
#18586=AXIS2_PLACEMENT_3D('',#28571,#22443,#22444);
#18587=AXIS2_PLACEMENT_3D('',#28573,#22445,#22446);
#18588=AXIS2_PLACEMENT_3D('',#28576,#22448,#22449);
#18589=AXIS2_PLACEMENT_3D('',#28578,#22450,#22451);
#18590=AXIS2_PLACEMENT_3D('',#28581,#22453,#22454);
#18591=AXIS2_PLACEMENT_3D('',#28583,#22455,#22456);
#18592=AXIS2_PLACEMENT_3D('',#28586,#22458,#22459);
#18593=AXIS2_PLACEMENT_3D('',#28588,#22460,#22461);
#18594=AXIS2_PLACEMENT_3D('',#28591,#22463,#22464);
#18595=AXIS2_PLACEMENT_3D('',#28593,#22465,#22466);
#18596=AXIS2_PLACEMENT_3D('',#28596,#22468,#22469);
#18597=AXIS2_PLACEMENT_3D('',#28599,#22471,#22472);
#18598=AXIS2_PLACEMENT_3D('',#28600,#22473,#22474);
#18599=AXIS2_PLACEMENT_3D('',#28601,#22475,#22476);
#18600=AXIS2_PLACEMENT_3D('',#28602,#22477,#22478);
#18601=AXIS2_PLACEMENT_3D('',#28633,#22480,#22481);
#18602=AXIS2_PLACEMENT_3D('',#28671,#22482,#22483);
#18603=AXIS2_PLACEMENT_3D('',#28758,#22485,#22486);
#18604=AXIS2_PLACEMENT_3D('',#28848,#22488,#22489);
#18605=AXIS2_PLACEMENT_3D('',#28935,#22491,#22492);
#18606=AXIS2_PLACEMENT_3D('',#29022,#22494,#22495);
#18607=AXIS2_PLACEMENT_3D('',#29112,#22497,#22498);
#18608=AXIS2_PLACEMENT_3D('',#29199,#22500,#22501);
#18609=AXIS2_PLACEMENT_3D('',#29286,#22503,#22504);
#18610=AXIS2_PLACEMENT_3D('',#29376,#22506,#22507);
#18611=AXIS2_PLACEMENT_3D('',#29463,#22509,#22510);
#18612=AXIS2_PLACEMENT_3D('',#29550,#22512,#22513);
#18613=AXIS2_PLACEMENT_3D('',#29563,#22515,#22516);
#18614=AXIS2_PLACEMENT_3D('',#29580,#22517,#22518);
#18615=AXIS2_PLACEMENT_3D('',#29598,#22520,#22521);
#18616=AXIS2_PLACEMENT_3D('',#29613,#22522,#22523);
#18617=AXIS2_PLACEMENT_3D('',#29650,#22525,#22526);
#18618=AXIS2_PLACEMENT_3D('',#29688,#22528,#22529);
#18619=AXIS2_PLACEMENT_3D('',#29725,#22531,#22532);
#18620=AXIS2_PLACEMENT_3D('',#29762,#22534,#22535);
#18621=AXIS2_PLACEMENT_3D('',#29800,#22537,#22538);
#18622=AXIS2_PLACEMENT_3D('',#29837,#22540,#22541);
#18623=AXIS2_PLACEMENT_3D('',#29874,#22543,#22544);
#18624=AXIS2_PLACEMENT_3D('',#29912,#22546,#22547);
#18625=AXIS2_PLACEMENT_3D('',#29949,#22549,#22550);
#18626=AXIS2_PLACEMENT_3D('',#29986,#22552,#22553);
#18627=AXIS2_PLACEMENT_3D('',#29998,#22555,#22556);
#18628=AXIS2_PLACEMENT_3D('',#30006,#22557,#22558);
#18629=AXIS2_PLACEMENT_3D('',#31877,#22559,#22560);
#18630=AXIS2_PLACEMENT_3D('',#31879,#22561,#22562);
#18631=AXIS2_PLACEMENT_3D('',#31880,#22563,#22564);
#18632=AXIS2_PLACEMENT_3D('',#31881,#22565,#22566);
#18633=AXIS2_PLACEMENT_3D('',#31883,#22567,#22568);
#18634=AXIS2_PLACEMENT_3D('',#31885,#22570,#22571);
#18635=AXIS2_PLACEMENT_3D('',#31887,#22572,#22573);
#18636=AXIS2_PLACEMENT_3D('',#31888,#22574,#22575);
#18637=AXIS2_PLACEMENT_3D('',#31890,#22576,#22577);
#18638=AXIS2_PLACEMENT_3D('',#31892,#22579,#22580);
#18639=AXIS2_PLACEMENT_3D('',#31894,#22581,#22582);
#18640=AXIS2_PLACEMENT_3D('',#31896,#22584,#22585);
#18641=AXIS2_PLACEMENT_3D('',#31897,#22586,#22587);
#18642=AXIS2_PLACEMENT_3D('',#31898,#22588,#22589);
#18643=AXIS2_PLACEMENT_3D('',#31914,#22591,#22592);
#18644=AXIS2_PLACEMENT_3D('',#31922,#22593,#22594);
#18645=AXIS2_PLACEMENT_3D('',#31970,#22596,#22597);
#18646=AXIS2_PLACEMENT_3D('',#32021,#22599,#22600);
#18647=AXIS2_PLACEMENT_3D('',#32072,#22602,#22603);
#18648=AXIS2_PLACEMENT_3D('',#32120,#22605,#22606);
#18649=AXIS2_PLACEMENT_3D('',#32174,#22608,#22609);
#18650=AXIS2_PLACEMENT_3D('',#32186,#22611,#22612);
#18651=AXIS2_PLACEMENT_3D('',#32192,#22613,#22614);
#18652=AXIS2_PLACEMENT_3D('',#32217,#22616,#22617);
#18653=AXIS2_PLACEMENT_3D('',#32242,#22619,#22620);
#18654=AXIS2_PLACEMENT_3D('',#32266,#22622,#22623);
#18655=AXIS2_PLACEMENT_3D('',#32292,#22625,#22626);
#18656=AXIS2_PLACEMENT_3D('',#32316,#22628,#22629);
#18657=AXIS2_PLACEMENT_3D('',#32407,#22630,#22631);
#18658=AXIS2_PLACEMENT_3D('',#32409,#22632,#22633);
#18659=AXIS2_PLACEMENT_3D('',#32800,#22634,#22635);
#18660=AXIS2_PLACEMENT_3D('',#32802,#22636,#22637);
#18661=AXIS2_PLACEMENT_3D('',#33100,#22638,#22639);
#18662=AXIS2_PLACEMENT_3D('',#33101,#22640,#22641);
#18663=AXIS2_PLACEMENT_3D('',#33102,#22642,#22643);
#18664=AXIS2_PLACEMENT_3D('',#33104,#22644,#22645);
#18665=AXIS2_PLACEMENT_3D('',#33105,#22646,#22647);
#18666=AXIS2_PLACEMENT_3D('',#33107,#22648,#22649);
#18667=AXIS2_PLACEMENT_3D('',#33109,#22651,#22652);
#18668=AXIS2_PLACEMENT_3D('',#33111,#22653,#22654);
#18669=AXIS2_PLACEMENT_3D('',#33113,#22656,#22657);
#18670=AXIS2_PLACEMENT_3D('',#33114,#22658,#22659);
#18671=AXIS2_PLACEMENT_3D('',#33116,#22660,#22661);
#18672=AXIS2_PLACEMENT_3D('',#33118,#22663,#22664);
#18673=AXIS2_PLACEMENT_3D('',#33119,#22665,#22666);
#18674=AXIS2_PLACEMENT_3D('',#33120,#22667,#22668);
#18675=AXIS2_PLACEMENT_3D('',#33123,#22669,#22670);
#18676=AXIS2_PLACEMENT_3D('',#33124,#22671,#22672);
#18677=AXIS2_PLACEMENT_3D('',#33128,#22674,#22675);
#18678=AXIS2_PLACEMENT_3D('',#33129,#22676,#22677);
#18679=AXIS2_PLACEMENT_3D('',#33130,#22678,#22679);
#18680=AXIS2_PLACEMENT_3D('',#33133,#22681,#22682);
#18681=AXIS2_PLACEMENT_3D('',#33134,#22683,#22684);
#18682=AXIS2_PLACEMENT_3D('',#33136,#22685,#22686);
#18683=AXIS2_PLACEMENT_3D('',#33138,#22688,#22689);
#18684=AXIS2_PLACEMENT_3D('',#33140,#22690,#22691);
#18685=AXIS2_PLACEMENT_3D('',#33142,#22692,#22693);
#18686=AXIS2_PLACEMENT_3D('',#33143,#22694,#22695);
#18687=AXIS2_PLACEMENT_3D('',#33146,#22697,#22698);
#18688=AXIS2_PLACEMENT_3D('',#33147,#22699,#22700);
#18689=AXIS2_PLACEMENT_3D('',#33150,#22702,#22703);
#18690=AXIS2_PLACEMENT_3D('',#33151,#22704,#22705);
#18691=AXIS2_PLACEMENT_3D('',#33152,#22706,#22707);
#18692=AXIS2_PLACEMENT_3D('',#33154,#22708,#22709);
#18693=AXIS2_PLACEMENT_3D('',#33157,#22711,#22712);
#18694=AXIS2_PLACEMENT_3D('',#33158,#22713,#22714);
#18695=AXIS2_PLACEMENT_3D('',#33160,#22715,#22716);
#18696=AXIS2_PLACEMENT_3D('',#33161,#22717,#22718);
#18697=AXIS2_PLACEMENT_3D('',#33163,#22720,#22721);
#18698=AXIS2_PLACEMENT_3D('',#33164,#22722,#22723);
#18699=AXIS2_PLACEMENT_3D('',#33165,#22724,#22725);
#18700=AXIS2_PLACEMENT_3D('',#33166,#22726,#22727);
#18701=AXIS2_PLACEMENT_3D('',#33168,#22728,#22729);
#18702=AXIS2_PLACEMENT_3D('',#33171,#22731,#22732);
#18703=AXIS2_PLACEMENT_3D('',#33172,#22733,#22734);
#18704=AXIS2_PLACEMENT_3D('',#33174,#22735,#22736);
#18705=AXIS2_PLACEMENT_3D('',#33175,#22737,#22738);
#18706=AXIS2_PLACEMENT_3D('',#33177,#22739,#22740);
#18707=AXIS2_PLACEMENT_3D('',#33179,#22742,#22743);
#18708=AXIS2_PLACEMENT_3D('',#33180,#22744,#22745);
#18709=AXIS2_PLACEMENT_3D('',#33181,#22746,#22747);
#18710=AXIS2_PLACEMENT_3D('',#33183,#22748,#22749);
#18711=AXIS2_PLACEMENT_3D('',#33187,#22751,#22752);
#18712=AXIS2_PLACEMENT_3D('',#33188,#22753,#22754);
#18713=AXIS2_PLACEMENT_3D('',#33189,#22755,#22756);
#18714=AXIS2_PLACEMENT_3D('',#33192,#22758,#22759);
#18715=AXIS2_PLACEMENT_3D('',#33193,#22760,#22761);
#18716=AXIS2_PLACEMENT_3D('',#33195,#22762,#22763);
#18717=AXIS2_PLACEMENT_3D('',#33196,#22764,#22765);
#18718=AXIS2_PLACEMENT_3D('',#33199,#22767,#22768);
#18719=AXIS2_PLACEMENT_3D('',#33200,#22769,#22770);
#18720=AXIS2_PLACEMENT_3D('',#33202,#22771,#22772);
#18721=AXIS2_PLACEMENT_3D('',#33203,#22773,#22774);
#18722=AXIS2_PLACEMENT_3D('',#33205,#22776,#22777);
#18723=AXIS2_PLACEMENT_3D('',#33206,#22778,#22779);
#18724=AXIS2_PLACEMENT_3D('',#33208,#22780,#22781);
#18725=AXIS2_PLACEMENT_3D('',#33211,#22783,#22784);
#18726=AXIS2_PLACEMENT_3D('',#33212,#22785,#22786);
#18727=AXIS2_PLACEMENT_3D('',#33215,#22788,#22789);
#18728=AXIS2_PLACEMENT_3D('',#33216,#22790,#22791);
#18729=AXIS2_PLACEMENT_3D('',#33218,#22792,#22793);
#18730=AXIS2_PLACEMENT_3D('',#33219,#22794,#22795);
#18731=AXIS2_PLACEMENT_3D('',#33221,#22796,#22797);
#18732=AXIS2_PLACEMENT_3D('',#33223,#22799,#22800);
#18733=AXIS2_PLACEMENT_3D('',#33225,#22801,#22802);
#18734=AXIS2_PLACEMENT_3D('',#33226,#22803,#22804);
#18735=AXIS2_PLACEMENT_3D('',#33250,#22806,#22807);
#18736=AXIS2_PLACEMENT_3D('',#33284,#22808,#22809);
#18737=AXIS2_PLACEMENT_3D('',#33318,#22810,#22811);
#18738=AXIS2_PLACEMENT_3D('',#33352,#22812,#22813);
#18739=AXIS2_PLACEMENT_3D('',#33386,#22814,#22815);
#18740=AXIS2_PLACEMENT_3D('',#33420,#22816,#22817);
#18741=AXIS2_PLACEMENT_3D('',#33534,#22818,#22819);
#18742=AXIS2_PLACEMENT_3D('',#33535,#22820,#22821);
#18743=AXIS2_PLACEMENT_3D('',#33540,#22822,#22823);
#18744=AXIS2_PLACEMENT_3D('',#33550,#22824,#22825);
#18745=AXIS2_PLACEMENT_3D('',#33560,#22826,#22827);
#18746=AXIS2_PLACEMENT_3D('',#33570,#22828,#22829);
#18747=AXIS2_PLACEMENT_3D('',#33614,#22830,#22831);
#18748=AXIS2_PLACEMENT_3D('',#33616,#22833,#22834);
#18749=AXIS2_PLACEMENT_3D('',#33625,#22836,#22837);
#18750=AXIS2_PLACEMENT_3D('',#33627,#22839,#22840);
#18751=AXIS2_PLACEMENT_3D('',#33643,#22842,#22843);
#18752=AXIS2_PLACEMENT_3D('',#33652,#22845,#22846);
#18753=AXIS2_PLACEMENT_3D('',#33693,#22848,#22849);
#18754=AXIS2_PLACEMENT_3D('',#33726,#22852,#22853);
#18755=AXIS2_PLACEMENT_3D('',#33734,#22856,#22857);
#18756=AXIS2_PLACEMENT_3D('',#33767,#22860,#22861);
#18757=AXIS2_PLACEMENT_3D('',#33775,#22864,#22865);
#18758=AXIS2_PLACEMENT_3D('',#33783,#22868,#22869);
#18759=AXIS2_PLACEMENT_3D('',#33791,#22872,#22873);
#18760=AXIS2_PLACEMENT_3D('',#33795,#22874,#22875);
#18761=AXIS2_PLACEMENT_3D('',#33799,#22876,#22877);
#18762=AXIS2_PLACEMENT_3D('',#33803,#22878,#22879);
#18763=AXIS2_PLACEMENT_3D('',#33818,#22881,#22882);
#18764=AXIS2_PLACEMENT_3D('',#33819,#22883,#22884);
#18765=AXIS2_PLACEMENT_3D('',#33820,#22885,#22886);
#18766=AXIS2_PLACEMENT_3D('',#33821,#22887,#22888);
#18767=AXIS2_PLACEMENT_3D('',#33822,#22889,#22890);
#18768=AXIS2_PLACEMENT_3D('',#33825,#22891,#22892);
#18769=AXIS2_PLACEMENT_3D('',#33826,#22893,#22894);
#18770=AXIS2_PLACEMENT_3D('',#34521,#22895,#22896);
#18771=AXIS2_PLACEMENT_3D('',#34586,#22897,#22898);
#18772=AXIS2_PLACEMENT_3D('',#34587,#22899,#22900);
#18773=AXIS2_PLACEMENT_3D('',#34588,#22901,#22902);
#18774=AXIS2_PLACEMENT_3D('',#34589,#22903,#22904);
#18775=AXIS2_PLACEMENT_3D('',#34590,#22905,#22906);
#18776=AXIS2_PLACEMENT_3D('',#34606,#22908,#22909);
#18777=AXIS2_PLACEMENT_3D('',#34614,#22910,#22911);
#18778=AXIS2_PLACEMENT_3D('',#34662,#22913,#22914);
#18779=AXIS2_PLACEMENT_3D('',#34710,#22916,#22917);
#18780=AXIS2_PLACEMENT_3D('',#34758,#22919,#22920);
#18781=AXIS2_PLACEMENT_3D('',#34771,#22922,#22923);
#18782=AXIS2_PLACEMENT_3D('',#34777,#22924,#22925);
#18783=AXIS2_PLACEMENT_3D('',#34802,#22927,#22928);
#18784=AXIS2_PLACEMENT_3D('',#34826,#22930,#22931);
#18785=AXIS2_PLACEMENT_3D('',#34850,#22933,#22934);
#18786=AXIS2_PLACEMENT_3D('',#34941,#22935,#22936);
#18787=AXIS2_PLACEMENT_3D('',#34943,#22937,#22938);
#18788=AXIS2_PLACEMENT_3D('',#35276,#22939,#22940);
#18789=AXIS2_PLACEMENT_3D('',#35278,#22941,#22942);
#18790=AXIS2_PLACEMENT_3D('',#35279,#22943,#22944);
#18791=AXIS2_PLACEMENT_3D('',#35369,#22945,#22946);
#18792=AXIS2_PLACEMENT_3D('',#35370,#22947,#22948);
#18793=AXIS2_PLACEMENT_3D('',#35522,#22949,#22950);
#18794=AXIS2_PLACEMENT_3D('',#35531,#22955,#22956);
#18795=AXIS2_PLACEMENT_3D('',#35537,#22960,#22961);
#18796=AXIS2_PLACEMENT_3D('',#35543,#22965,#22966);
#18797=AXIS2_PLACEMENT_3D('',#35549,#22970,#22971);
#18798=AXIS2_PLACEMENT_3D('',#35555,#22975,#22976);
#18799=AXIS2_PLACEMENT_3D('',#35558,#22979,#22980);
#18800=AXIS2_PLACEMENT_3D('',#35559,#22981,#22982);
#18801=AXIS2_PLACEMENT_3D('',#35561,#22983,#22984);
#18802=AXIS2_PLACEMENT_3D('',#35562,#22985,#22986);
#18803=AXIS2_PLACEMENT_3D('',#35564,#22988,#22989);
#18804=AXIS2_PLACEMENT_3D('',#35565,#22990,#22991);
#18805=AXIS2_PLACEMENT_3D('',#35566,#22992,#22993);
#18806=AXIS2_PLACEMENT_3D('',#35568,#22994,#22995);
#18807=AXIS2_PLACEMENT_3D('',#35570,#22997,#22998);
#18808=AXIS2_PLACEMENT_3D('',#35571,#22999,#23000);
#18809=AXIS2_PLACEMENT_3D('',#35572,#23001,#23002);
#18810=AXIS2_PLACEMENT_3D('',#35588,#23004,#23005);
#18811=AXIS2_PLACEMENT_3D('',#35596,#23006,#23007);
#18812=AXIS2_PLACEMENT_3D('',#35644,#23009,#23010);
#18813=AXIS2_PLACEMENT_3D('',#35692,#23012,#23013);
#18814=AXIS2_PLACEMENT_3D('',#35746,#23015,#23016);
#18815=AXIS2_PLACEMENT_3D('',#35794,#23018,#23019);
#18816=AXIS2_PLACEMENT_3D('',#35842,#23021,#23022);
#18817=AXIS2_PLACEMENT_3D('',#35890,#23024,#23025);
#18818=AXIS2_PLACEMENT_3D('',#35944,#23027,#23028);
#18819=AXIS2_PLACEMENT_3D('',#35992,#23030,#23031);
#18820=AXIS2_PLACEMENT_3D('',#36040,#23033,#23034);
#18821=AXIS2_PLACEMENT_3D('',#36094,#23036,#23037);
#18822=AXIS2_PLACEMENT_3D('',#36142,#23039,#23040);
#18823=AXIS2_PLACEMENT_3D('',#36190,#23042,#23043);
#18824=AXIS2_PLACEMENT_3D('',#36244,#23045,#23046);
#18825=AXIS2_PLACEMENT_3D('',#36292,#23048,#23049);
#18826=AXIS2_PLACEMENT_3D('',#36307,#23051,#23052);
#18827=AXIS2_PLACEMENT_3D('',#36316,#23053,#23054);
#18828=AXIS2_PLACEMENT_3D('',#36341,#23056,#23057);
#18829=AXIS2_PLACEMENT_3D('',#36366,#23059,#23060);
#18830=AXIS2_PLACEMENT_3D('',#36390,#23062,#23063);
#18831=AXIS2_PLACEMENT_3D('',#36415,#23065,#23066);
#18832=AXIS2_PLACEMENT_3D('',#36440,#23068,#23069);
#18833=AXIS2_PLACEMENT_3D('',#36464,#23071,#23072);
#18834=AXIS2_PLACEMENT_3D('',#36489,#23074,#23075);
#18835=AXIS2_PLACEMENT_3D('',#36514,#23077,#23078);
#18836=AXIS2_PLACEMENT_3D('',#36538,#23080,#23081);
#18837=AXIS2_PLACEMENT_3D('',#36562,#23083,#23084);
#18838=AXIS2_PLACEMENT_3D('',#36587,#23086,#23087);
#18839=AXIS2_PLACEMENT_3D('',#36612,#23089,#23090);
#18840=AXIS2_PLACEMENT_3D('',#37218,#23092,#23093);
#18841=AXIS2_PLACEMENT_3D('',#37220,#23094,#23095);
#18842=AXIS2_PLACEMENT_3D('',#37221,#23096,#23097);
#18843=AXIS2_PLACEMENT_3D('',#37311,#23098,#23099);
#18844=AXIS2_PLACEMENT_3D('',#37312,#23100,#23101);
#18845=AXIS2_PLACEMENT_3D('',#37802,#23102,#23103);
#18846=AXIS2_PLACEMENT_3D('',#37813,#23107,#23108);
#18847=AXIS2_PLACEMENT_3D('',#37815,#23109,#23110);
#18848=AXIS2_PLACEMENT_3D('',#37817,#23112,#23113);
#18849=AXIS2_PLACEMENT_3D('',#37823,#23115,#23116);
#18850=AXIS2_PLACEMENT_3D('',#37825,#23117,#23118);
#18851=AXIS2_PLACEMENT_3D('',#37829,#23120,#23121);
#18852=AXIS2_PLACEMENT_3D('',#37833,#23123,#23124);
#18853=AXIS2_PLACEMENT_3D('',#37837,#23126,#23127);
#18854=AXIS2_PLACEMENT_3D('',#37841,#23129,#23130);
#18855=AXIS2_PLACEMENT_3D('',#37845,#23132,#23133);
#18856=AXIS2_PLACEMENT_3D('',#37849,#23135,#23136);
#18857=AXIS2_PLACEMENT_3D('',#37853,#23138,#23139);
#18858=AXIS2_PLACEMENT_3D('',#37857,#23141,#23142);
#18859=AXIS2_PLACEMENT_3D('',#37861,#23144,#23145);
#18860=AXIS2_PLACEMENT_3D('',#37865,#23147,#23148);
#18861=AXIS2_PLACEMENT_3D('',#37869,#23150,#23151);
#18862=AXIS2_PLACEMENT_3D('',#37873,#23153,#23154);
#18863=AXIS2_PLACEMENT_3D('',#37877,#23156,#23157);
#18864=AXIS2_PLACEMENT_3D('',#37881,#23159,#23160);
#18865=AXIS2_PLACEMENT_3D('',#37885,#23162,#23163);
#18866=AXIS2_PLACEMENT_3D('',#37889,#23165,#23166);
#18867=AXIS2_PLACEMENT_3D('',#37893,#23168,#23169);
#18868=AXIS2_PLACEMENT_3D('',#37897,#23171,#23172);
#18869=AXIS2_PLACEMENT_3D('',#37901,#23174,#23175);
#18870=AXIS2_PLACEMENT_3D('',#37905,#23177,#23178);
#18871=AXIS2_PLACEMENT_3D('',#37909,#23180,#23181);
#18872=AXIS2_PLACEMENT_3D('',#37913,#23183,#23184);
#18873=AXIS2_PLACEMENT_3D('',#37917,#23186,#23187);
#18874=AXIS2_PLACEMENT_3D('',#37921,#23189,#23190);
#18875=AXIS2_PLACEMENT_3D('',#37925,#23192,#23193);
#18876=AXIS2_PLACEMENT_3D('',#37929,#23195,#23196);
#18877=AXIS2_PLACEMENT_3D('',#37933,#23198,#23199);
#18878=AXIS2_PLACEMENT_3D('',#37936,#23201,#23202);
#18879=AXIS2_PLACEMENT_3D('',#37938,#23203,#23204);
#18880=AXIS2_PLACEMENT_3D('',#37942,#23206,#23207);
#18881=AXIS2_PLACEMENT_3D('',#37946,#23209,#23210);
#18882=AXIS2_PLACEMENT_3D('',#37950,#23212,#23213);
#18883=AXIS2_PLACEMENT_3D('',#37954,#23215,#23216);
#18884=AXIS2_PLACEMENT_3D('',#37958,#23218,#23219);
#18885=AXIS2_PLACEMENT_3D('',#37962,#23221,#23222);
#18886=AXIS2_PLACEMENT_3D('',#37966,#23224,#23225);
#18887=AXIS2_PLACEMENT_3D('',#37970,#23227,#23228);
#18888=AXIS2_PLACEMENT_3D('',#37974,#23230,#23231);
#18889=AXIS2_PLACEMENT_3D('',#37978,#23233,#23234);
#18890=AXIS2_PLACEMENT_3D('',#37982,#23236,#23237);
#18891=AXIS2_PLACEMENT_3D('',#37986,#23239,#23240);
#18892=AXIS2_PLACEMENT_3D('',#37990,#23242,#23243);
#18893=AXIS2_PLACEMENT_3D('',#37994,#23245,#23246);
#18894=AXIS2_PLACEMENT_3D('',#37998,#23248,#23249);
#18895=AXIS2_PLACEMENT_3D('',#38002,#23251,#23252);
#18896=AXIS2_PLACEMENT_3D('',#38006,#23254,#23255);
#18897=AXIS2_PLACEMENT_3D('',#38010,#23257,#23258);
#18898=AXIS2_PLACEMENT_3D('',#38014,#23260,#23261);
#18899=AXIS2_PLACEMENT_3D('',#38018,#23263,#23264);
#18900=AXIS2_PLACEMENT_3D('',#38022,#23266,#23267);
#18901=AXIS2_PLACEMENT_3D('',#38026,#23269,#23270);
#18902=AXIS2_PLACEMENT_3D('',#38030,#23272,#23273);
#18903=AXIS2_PLACEMENT_3D('',#38034,#23275,#23276);
#18904=AXIS2_PLACEMENT_3D('',#38038,#23278,#23279);
#18905=AXIS2_PLACEMENT_3D('',#38042,#23281,#23282);
#18906=AXIS2_PLACEMENT_3D('',#38046,#23284,#23285);
#18907=AXIS2_PLACEMENT_3D('',#38050,#23287,#23288);
#18908=AXIS2_PLACEMENT_3D('',#38054,#23290,#23291);
#18909=AXIS2_PLACEMENT_3D('',#38058,#23293,#23294);
#18910=AXIS2_PLACEMENT_3D('',#38061,#23296,#23297);
#18911=AXIS2_PLACEMENT_3D('',#38062,#23298,#23299);
#18912=AXIS2_PLACEMENT_3D('',#38070,#23302,#23303);
#18913=AXIS2_PLACEMENT_3D('',#38072,#23305,#23306);
#18914=AXIS2_PLACEMENT_3D('',#38076,#23307,#23308);
#18915=AXIS2_PLACEMENT_3D('',#38084,#23311,#23312);
#18916=AXIS2_PLACEMENT_3D('',#38086,#23314,#23315);
#18917=AXIS2_PLACEMENT_3D('',#38090,#23316,#23317);
#18918=AXIS2_PLACEMENT_3D('',#38098,#23320,#23321);
#18919=AXIS2_PLACEMENT_3D('',#38100,#23323,#23324);
#18920=AXIS2_PLACEMENT_3D('',#38104,#23325,#23326);
#18921=AXIS2_PLACEMENT_3D('',#38112,#23329,#23330);
#18922=AXIS2_PLACEMENT_3D('',#38114,#23332,#23333);
#18923=AXIS2_PLACEMENT_3D('',#38118,#23334,#23335);
#18924=AXIS2_PLACEMENT_3D('',#38126,#23338,#23339);
#18925=AXIS2_PLACEMENT_3D('',#38128,#23341,#23342);
#18926=AXIS2_PLACEMENT_3D('',#38132,#23343,#23344);
#18927=AXIS2_PLACEMENT_3D('',#38140,#23347,#23348);
#18928=AXIS2_PLACEMENT_3D('',#38142,#23350,#23351);
#18929=AXIS2_PLACEMENT_3D('',#38146,#23352,#23353);
#18930=AXIS2_PLACEMENT_3D('',#38154,#23356,#23357);
#18931=AXIS2_PLACEMENT_3D('',#38156,#23359,#23360);
#18932=AXIS2_PLACEMENT_3D('',#38160,#23361,#23362);
#18933=AXIS2_PLACEMENT_3D('',#38168,#23365,#23366);
#18934=AXIS2_PLACEMENT_3D('',#38170,#23368,#23369);
#18935=AXIS2_PLACEMENT_3D('',#38174,#23370,#23371);
#18936=AXIS2_PLACEMENT_3D('',#38182,#23374,#23375);
#18937=AXIS2_PLACEMENT_3D('',#38184,#23377,#23378);
#18938=AXIS2_PLACEMENT_3D('',#38188,#23379,#23380);
#18939=AXIS2_PLACEMENT_3D('',#38196,#23383,#23384);
#18940=AXIS2_PLACEMENT_3D('',#38198,#23386,#23387);
#18941=AXIS2_PLACEMENT_3D('',#38202,#23388,#23389);
#18942=AXIS2_PLACEMENT_3D('',#38210,#23392,#23393);
#18943=AXIS2_PLACEMENT_3D('',#38212,#23395,#23396);
#18944=AXIS2_PLACEMENT_3D('',#38216,#23397,#23398);
#18945=AXIS2_PLACEMENT_3D('',#38224,#23401,#23402);
#18946=AXIS2_PLACEMENT_3D('',#38226,#23404,#23405);
#18947=AXIS2_PLACEMENT_3D('',#38230,#23406,#23407);
#18948=AXIS2_PLACEMENT_3D('',#38238,#23410,#23411);
#18949=AXIS2_PLACEMENT_3D('',#38240,#23413,#23414);
#18950=AXIS2_PLACEMENT_3D('',#38244,#23415,#23416);
#18951=AXIS2_PLACEMENT_3D('',#38252,#23419,#23420);
#18952=AXIS2_PLACEMENT_3D('',#38254,#23422,#23423);
#18953=AXIS2_PLACEMENT_3D('',#38258,#23424,#23425);
#18954=AXIS2_PLACEMENT_3D('',#38266,#23428,#23429);
#18955=AXIS2_PLACEMENT_3D('',#38268,#23431,#23432);
#18956=AXIS2_PLACEMENT_3D('',#38272,#23433,#23434);
#18957=AXIS2_PLACEMENT_3D('',#38280,#23437,#23438);
#18958=AXIS2_PLACEMENT_3D('',#38282,#23440,#23441);
#18959=AXIS2_PLACEMENT_3D('',#38286,#23442,#23443);
#18960=AXIS2_PLACEMENT_3D('',#38294,#23446,#23447);
#18961=AXIS2_PLACEMENT_3D('',#38296,#23449,#23450);
#18962=AXIS2_PLACEMENT_3D('',#38300,#23451,#23452);
#18963=AXIS2_PLACEMENT_3D('',#38308,#23455,#23456);
#18964=AXIS2_PLACEMENT_3D('',#38310,#23458,#23459);
#18965=AXIS2_PLACEMENT_3D('',#38314,#23460,#23461);
#18966=AXIS2_PLACEMENT_3D('',#38322,#23464,#23465);
#18967=AXIS2_PLACEMENT_3D('',#38324,#23467,#23468);
#18968=AXIS2_PLACEMENT_3D('',#38328,#23469,#23470);
#18969=AXIS2_PLACEMENT_3D('',#38336,#23473,#23474);
#18970=AXIS2_PLACEMENT_3D('',#38338,#23476,#23477);
#18971=AXIS2_PLACEMENT_3D('',#38342,#23478,#23479);
#18972=AXIS2_PLACEMENT_3D('',#38350,#23482,#23483);
#18973=AXIS2_PLACEMENT_3D('',#38352,#23485,#23486);
#18974=AXIS2_PLACEMENT_3D('',#38356,#23487,#23488);
#18975=AXIS2_PLACEMENT_3D('',#38364,#23491,#23492);
#18976=AXIS2_PLACEMENT_3D('',#38366,#23494,#23495);
#18977=AXIS2_PLACEMENT_3D('',#38370,#23496,#23497);
#18978=AXIS2_PLACEMENT_3D('',#38378,#23500,#23501);
#18979=AXIS2_PLACEMENT_3D('',#38380,#23503,#23504);
#18980=AXIS2_PLACEMENT_3D('',#38384,#23505,#23506);
#18981=AXIS2_PLACEMENT_3D('',#38392,#23509,#23510);
#18982=AXIS2_PLACEMENT_3D('',#38394,#23512,#23513);
#18983=AXIS2_PLACEMENT_3D('',#38398,#23514,#23515);
#18984=AXIS2_PLACEMENT_3D('',#38406,#23518,#23519);
#18985=AXIS2_PLACEMENT_3D('',#38408,#23521,#23522);
#18986=AXIS2_PLACEMENT_3D('',#38412,#23523,#23524);
#18987=AXIS2_PLACEMENT_3D('',#38420,#23527,#23528);
#18988=AXIS2_PLACEMENT_3D('',#38422,#23530,#23531);
#18989=AXIS2_PLACEMENT_3D('',#38426,#23532,#23533);
#18990=AXIS2_PLACEMENT_3D('',#38434,#23536,#23537);
#18991=AXIS2_PLACEMENT_3D('',#38436,#23539,#23540);
#18992=AXIS2_PLACEMENT_3D('',#38440,#23541,#23542);
#18993=AXIS2_PLACEMENT_3D('',#38448,#23545,#23546);
#18994=AXIS2_PLACEMENT_3D('',#38450,#23548,#23549);
#18995=AXIS2_PLACEMENT_3D('',#38454,#23550,#23551);
#18996=AXIS2_PLACEMENT_3D('',#38462,#23554,#23555);
#18997=AXIS2_PLACEMENT_3D('',#38464,#23557,#23558);
#18998=AXIS2_PLACEMENT_3D('',#38468,#23559,#23560);
#18999=AXIS2_PLACEMENT_3D('',#38470,#23561,#23562);
#19000=AXIS2_PLACEMENT_3D('',#38471,#23563,#23564);
#19001=AXIS2_PLACEMENT_3D('',#38473,#23566,#23567);
#19002=AXIS2_PLACEMENT_3D('',#38474,#23568,#23569);
#19003=AXIS2_PLACEMENT_3D('',#38475,#23570,#23571);
#19004=AXIS2_PLACEMENT_3D('',#38477,#23572,#23573);
#19005=AXIS2_PLACEMENT_3D('',#38478,#23574,#23575);
#19006=AXIS2_PLACEMENT_3D('',#38480,#23577,#23578);
#19007=AXIS2_PLACEMENT_3D('',#38482,#23579,#23580);
#19008=AXIS2_PLACEMENT_3D('',#38484,#23582,#23583);
#19009=AXIS2_PLACEMENT_3D('',#38485,#23584,#23585);
#19010=AXIS2_PLACEMENT_3D('',#38486,#23586,#23587);
#19011=AXIS2_PLACEMENT_3D('',#38487,#23588,#23589);
#19012=AXIS2_PLACEMENT_3D('',#38488,#23590,#23591);
#19013=AXIS2_PLACEMENT_3D('',#38489,#23592,#23593);
#19014=AXIS2_PLACEMENT_3D('',#38490,#23594,#23595);
#19015=AXIS2_PLACEMENT_3D('',#38491,#23596,#23597);
#19016=AXIS2_PLACEMENT_3D('',#38492,#23598,#23599);
#19017=AXIS2_PLACEMENT_3D('',#38493,#23600,#23601);
#19018=AXIS2_PLACEMENT_3D('',#38494,#23602,#23603);
#19019=AXIS2_PLACEMENT_3D('',#38495,#23604,#23605);
#19020=AXIS2_PLACEMENT_3D('',#38496,#23606,#23607);
#19021=AXIS2_PLACEMENT_3D('',#38497,#23608,#23609);
#19022=AXIS2_PLACEMENT_3D('',#38498,#23610,#23611);
#19023=AXIS2_PLACEMENT_3D('',#38499,#23612,#23613);
#19024=AXIS2_PLACEMENT_3D('',#38500,#23614,#23615);
#19025=DIRECTION('axis',(0.,0.,1.));
#19026=DIRECTION('refdir',(1.,0.,0.));
#19027=DIRECTION('axis',(0.,0.,1.));
#19028=DIRECTION('refdir',(1.,0.,0.));
#19029=DIRECTION('center_axis',(0.,-0.707106781186548,0.707106781186548));
#19030=DIRECTION('ref_axis',(1.,0.,0.));
#19031=DIRECTION('',(-1.,0.,0.));
#19032=DIRECTION('',(0.577350269189631,-0.577350269189623,-0.577350269189623));
#19033=DIRECTION('',(1.,0.,0.));
#19034=DIRECTION('',(-0.577350269189631,-0.577350269189623,-0.577350269189623));
#19035=DIRECTION('center_axis',(0.,0.707106781186549,0.707106781186546));
#19036=DIRECTION('ref_axis',(1.,0.,0.));
#19037=DIRECTION('',(1.,0.,0.));
#19038=DIRECTION('',(-0.577350269189632,0.577350269189622,-0.577350269189624));
#19039=DIRECTION('',(-1.,0.,0.));
#19040=DIRECTION('',(-0.577350269189632,-0.577350269189622,0.577350269189624));
#19041=DIRECTION('center_axis',(-0.707106781186543,0.,0.707106781186552));
#19042=DIRECTION('ref_axis',(0.707106781186552,0.,0.707106781186543));
#19043=DIRECTION('',(0.,-1.,0.));
#19044=DIRECTION('',(0.,1.,0.));
#19045=DIRECTION('center_axis',(0.707106781186543,0.,0.707106781186552));
#19046=DIRECTION('ref_axis',(0.707106781186552,0.,-0.707106781186543));
#19047=DIRECTION('',(0.,-1.,0.));
#19048=DIRECTION('',(0.,1.,0.));
#19049=DIRECTION('center_axis',(-1.,0.,0.));
#19050=DIRECTION('ref_axis',(0.,1.,0.));
#19051=DIRECTION('',(0.,0.,-1.));
#19052=DIRECTION('',(0.,1.,0.));
#19053=DIRECTION('',(0.,0.,-1.));
#19054=DIRECTION('center_axis',(0.,-1.,0.));
#19055=DIRECTION('ref_axis',(-1.,0.,0.));
#19056=DIRECTION('',(0.,0.,-1.));
#19057=DIRECTION('',(-1.,0.,0.));
#19058=DIRECTION('center_axis',(0.,0.,1.));
#19059=DIRECTION('ref_axis',(0.,1.,0.));
#19060=DIRECTION('',(1.,0.,0.));
#19061=DIRECTION('',(0.,1.,0.));
#19062=DIRECTION('',(-1.,0.,0.));
#19063=DIRECTION('center_axis',(0.,0.,1.));
#19064=DIRECTION('ref_axis',(1.,0.,0.));
#19065=DIRECTION('center_axis',(0.,0.,1.));
#19066=DIRECTION('ref_axis',(1.,0.,0.));
#19067=DIRECTION('',(-1.,0.,0.));
#19068=DIRECTION('',(0.,1.,0.));
#19069=DIRECTION('',(1.,0.,0.));
#19070=DIRECTION('',(0.,-1.,0.));
#19071=DIRECTION('',(-1.,0.,0.));
#19072=DIRECTION('',(0.,1.,0.));
#19073=DIRECTION('',(1.,0.,0.));
#19074=DIRECTION('',(0.,-1.,0.));
#19075=DIRECTION('',(1.,0.,0.));
#19076=DIRECTION('',(0.,-1.,0.));
#19077=DIRECTION('',(-1.,0.,0.));
#19078=DIRECTION('',(0.,1.,0.));
#19079=DIRECTION('center_axis',(-0.707106781186549,0.,0.707106781186546));
#19080=DIRECTION('ref_axis',(0.707106781186546,0.,0.707106781186549));
#19081=DIRECTION('',(0.,-1.,0.));
#19082=DIRECTION('',(-0.577350269189623,0.577350269189628,-0.577350269189626));
#19083=DIRECTION('',(-0.577350269189625,-0.577350269189625,-0.577350269189627));
#19084=DIRECTION('center_axis',(0.,-0.707106781186549,0.707106781186546));
#19085=DIRECTION('ref_axis',(1.,0.,0.));
#19086=DIRECTION('',(1.,0.,0.));
#19087=DIRECTION('',(0.577350269189618,-0.577350269189629,-0.577350269189631));
#19088=DIRECTION('center_axis',(0.707106781186555,0.,0.70710678118654));
#19089=DIRECTION('ref_axis',(0.70710678118654,0.,-0.707106781186555));
#19090=DIRECTION('',(-0.577350269189616,-0.577350269189632,0.577350269189629));
#19091=DIRECTION('',(0.,1.,0.));
#19092=DIRECTION('center_axis',(1.,0.,0.));
#19093=DIRECTION('ref_axis',(0.,-1.,0.));
#19094=DIRECTION('',(0.,0.,-1.));
#19095=DIRECTION('',(0.,-1.,0.));
#19096=DIRECTION('',(0.,0.,-1.));
#19097=DIRECTION('center_axis',(0.,1.,0.));
#19098=DIRECTION('ref_axis',(1.,0.,0.));
#19099=DIRECTION('',(0.,0.,-1.));
#19100=DIRECTION('',(1.,0.,0.));
#19101=DIRECTION('center_axis',(-1.,0.,0.));
#19102=DIRECTION('ref_axis',(0.,1.,0.));
#19103=DIRECTION('',(0.,0.,-1.));
#19104=DIRECTION('',(0.,1.,0.));
#19105=DIRECTION('center_axis',(0.707106781186555,0.,0.70710678118654));
#19106=DIRECTION('ref_axis',(0.70710678118654,0.,-0.707106781186555));
#19107=DIRECTION('',(-0.577350269189618,-0.577350269189629,0.577350269189631));
#19108=DIRECTION('',(0.,1.,0.));
#19109=DIRECTION('',(0.577350269189617,-0.57735026918963,-0.57735026918963));
#19110=DIRECTION('center_axis',(-1.,0.,0.));
#19111=DIRECTION('ref_axis',(0.,1.,0.));
#19112=DIRECTION('',(0.,0.,-1.));
#19113=DIRECTION('',(0.,1.,0.));
#19114=DIRECTION('',(0.,0.,-1.));
#19115=DIRECTION('center_axis',(-0.707106781186549,0.,0.707106781186546));
#19116=DIRECTION('ref_axis',(0.707106781186546,0.,0.707106781186549));
#19117=DIRECTION('',(0.577350269189624,0.577350269189627,0.577350269189627));
#19118=DIRECTION('',(0.,-1.,0.));
#19119=DIRECTION('',(-0.577350269189625,0.577350269189625,-0.577350269189627));
#19120=DIRECTION('center_axis',(1.,0.,0.));
#19121=DIRECTION('ref_axis',(0.,-1.,0.));
#19122=DIRECTION('',(0.,0.,-1.));
#19123=DIRECTION('',(0.,-1.,0.));
#19124=DIRECTION('',(0.,0.,-1.));
#19125=DIRECTION('center_axis',(0.707106781186543,0.,0.707106781186552));
#19126=DIRECTION('ref_axis',(0.707106781186552,0.,-0.707106781186543));
#19127=DIRECTION('',(-0.57735026918963,-0.577350269189625,0.577350269189622));
#19128=DIRECTION('',(0.,1.,0.));
#19129=DIRECTION('',(0.577350269189632,-0.577350269189622,-0.577350269189624));
#19130=DIRECTION('center_axis',(-1.,0.,0.));
#19131=DIRECTION('ref_axis',(0.,1.,0.));
#19132=DIRECTION('',(0.,0.,-1.));
#19133=DIRECTION('',(0.,1.,0.));
#19134=DIRECTION('',(0.,0.,-1.));
#19135=DIRECTION('center_axis',(-0.707106781186543,0.,0.707106781186552));
#19136=DIRECTION('ref_axis',(0.707106781186552,0.,0.707106781186543));
#19137=DIRECTION('',(0.577350269189632,0.577350269189622,0.577350269189624));
#19138=DIRECTION('',(0.,-1.,0.));
#19139=DIRECTION('',(-0.57735026918963,0.577350269189625,-0.577350269189622));
#19140=DIRECTION('center_axis',(1.,0.,0.));
#19141=DIRECTION('ref_axis',(0.,-1.,0.));
#19142=DIRECTION('',(0.,0.,-1.));
#19143=DIRECTION('',(0.,-1.,0.));
#19144=DIRECTION('',(0.,0.,-1.));
#19145=DIRECTION('center_axis',(-0.750023489558556,-0.572798894755224,0.330705596078447));
#19146=DIRECTION('ref_axis',(0.403449110677542,0.,0.915002084748172));
#19147=DIRECTION('',(-0.627963030199562,0.773682358480754,-0.0841310934092862));
#19148=DIRECTION('',(0.,-0.499999999999999,-0.866025403784439));
#19149=DIRECTION('',(0.627963030199561,-0.459700843380977,0.627963030199552));
#19150=DIRECTION('center_axis',(0.,-0.866025403784439,0.499999999999999));
#19151=DIRECTION('ref_axis',(0.,-0.499999999999999,-0.866025403784439));
#19152=DIRECTION('center_axis',(0.,-0.866025403784439,0.499999999999999));
#19153=DIRECTION('ref_axis',(0.,0.499999999999999,0.866025403784439));
#19154=DIRECTION('',(1.,0.,0.));
#19155=DIRECTION('center_axis',(-0.750023489558558,0.572798894755222,0.330705596078446));
#19156=DIRECTION('ref_axis',(0.40344911067754,0.,0.915002084748173));
#19157=DIRECTION('',(-0.627963030199559,-0.459700843380982,-0.627963030199551));
#19158=DIRECTION('',(0.,-0.499999999999999,0.866025403784439));
#19159=DIRECTION('',(0.627963030199559,0.773682358480756,0.0841310934092859));
#19160=DIRECTION('center_axis',(0.,0.866025403784439,0.499999999999999));
#19161=DIRECTION('ref_axis',(0.,-0.499999999999999,0.866025403784439));
#19162=DIRECTION('center_axis',(0.,0.866025403784439,0.499999999999999));
#19163=DIRECTION('ref_axis',(0.,0.499999999999999,-0.866025403784439));
#19164=DIRECTION('',(-1.,0.,0.));
#19165=DIRECTION('center_axis',(-0.707106781186544,0.612372435695797,-0.353553390593276));
#19166=DIRECTION('ref_axis',(-0.447213595499961,0.,0.894427190999914));
#19167=DIRECTION('',(-0.654653670707978,-0.37796447300922,0.65465367070798));
#19168=DIRECTION('',(0.,0.5,0.866025403784439));
#19169=DIRECTION('',(0.,-0.5,-0.866025403784439));
#19170=DIRECTION('',(-0.447213595499962,-0.774596669241483,-0.447213595499955));
#19171=DIRECTION('center_axis',(-0.707106781186543,0.,0.707106781186552));
#19172=DIRECTION('ref_axis',(0.707106781186552,0.,0.707106781186543));
#19173=DIRECTION('',(0.,-1.,0.));
#19174=DIRECTION('center_axis',(-0.707106781186541,-0.6123724356958,-0.353553390593277));
#19175=DIRECTION('ref_axis',(-0.447213595499965,0.,0.894427190999912));
#19176=DIRECTION('',(0.447213595499965,-0.774596669241481,0.447213595499956));
#19177=DIRECTION('',(0.,-0.5,0.866025403784439));
#19178=DIRECTION('',(0.,0.5,-0.866025403784439));
#19179=DIRECTION('',(0.65465367070798,-0.377964473009213,-0.654653670707982));
#19180=DIRECTION('center_axis',(0.,-0.866025403784439,-0.5));
#19181=DIRECTION('ref_axis',(0.,-0.5,0.866025403784439));
#19182=DIRECTION('',(-1.,0.,0.));
#19183=DIRECTION('center_axis',(0.,-0.866025403784439,-0.5));
#19184=DIRECTION('ref_axis',(0.,0.5,-0.866025403784439));
#19185=DIRECTION('center_axis',(0.,-0.5,-0.866025403784439));
#19186=DIRECTION('ref_axis',(-1.,0.,0.));
#19187=DIRECTION('',(-0.447213595499957,-0.774596669241484,0.447213595499958));
#19188=DIRECTION('',(1.,0.,0.));
#19189=DIRECTION('center_axis',(0.,0.5,0.866025403784439));
#19190=DIRECTION('ref_axis',(-2.8028386894984E-15,0.866025403784439,-0.5));
#19191=DIRECTION('center_axis',(0.,0.,1.));
#19192=DIRECTION('ref_axis',(1.,0.,0.));
#19193=DIRECTION('center_axis',(0.,0.,-1.));
#19194=DIRECTION('ref_axis',(1.,0.,0.));
#19195=DIRECTION('center_axis',(0.,0.,1.));
#19196=DIRECTION('ref_axis',(1.,0.,0.));
#19197=DIRECTION('center_axis',(0.,-1.,0.));
#19198=DIRECTION('ref_axis',(5.0532154980743E-16,0.,1.));
#19199=DIRECTION('',(0.,1.,0.));
#19200=DIRECTION('center_axis',(0.,-0.707106781186549,0.707106781186546));
#19201=DIRECTION('ref_axis',(0.,0.707106781186546,0.707106781186549));
#19202=DIRECTION('center_axis',(0.,-1.,0.));
#19203=DIRECTION('ref_axis',(1.,0.,0.));
#19204=DIRECTION('center_axis',(0.,-0.707106781186549,0.707106781186546));
#19205=DIRECTION('ref_axis',(0.,0.707106781186546,0.707106781186549));
#19206=DIRECTION('',(0.,-1.,0.));
#19207=DIRECTION('center_axis',(0.,0.,1.));
#19208=DIRECTION('ref_axis',(1.,0.,0.));
#19209=DIRECTION('',(0.,-1.,0.));
#19210=DIRECTION('',(-1.,0.,0.));
#19211=DIRECTION('center_axis',(0.,0.,1.));
#19212=DIRECTION('ref_axis',(-1.,0.,0.));
#19213=DIRECTION('',(-1.,0.,0.));
#19214=DIRECTION('center_axis',(0.,0.,-1.));
#19215=DIRECTION('ref_axis',(1.,0.,0.));
#19216=DIRECTION('center_axis',(0.,0.,-1.));
#19217=DIRECTION('ref_axis',(1.,0.,0.));
#19218=DIRECTION('center_axis',(0.,0.,1.));
#19219=DIRECTION('ref_axis',(-1.,0.,0.));
#19220=DIRECTION('center_axis',(0.,0.,-1.));
#19221=DIRECTION('ref_axis',(-1.,0.,0.));
#19222=DIRECTION('center_axis',(0.,-0.499999999999998,0.86602540378444));
#19223=DIRECTION('ref_axis',(3.93732101620015E-15,0.86602540378444,0.499999999999998));
#19224=DIRECTION('center_axis',(0.,0.707106781186546,0.707106781186549));
#19225=DIRECTION('ref_axis',(1.,0.,0.));
#19226=DIRECTION('',(-1.,0.,0.));
#19227=DIRECTION('center_axis',(0.,-1.,0.));
#19228=DIRECTION('ref_axis',(-1.,0.,0.));
#19229=DIRECTION('',(-1.,0.,0.));
#19230=DIRECTION('center_axis',(0.,-0.707106781186548,0.707106781186548));
#19231=DIRECTION('ref_axis',(1.,0.,0.));
#19232=DIRECTION('',(1.,0.,0.));
#19233=DIRECTION('center_axis',(0.,1.,0.));
#19234=DIRECTION('ref_axis',(1.,0.,0.));
#19235=DIRECTION('',(1.,0.,0.));
#19236=DIRECTION('center_axis',(0.,0.707106781186549,0.707106781186546));
#19237=DIRECTION('ref_axis',(1.,0.,0.));
#19238=DIRECTION('',(-1.,0.,0.));
#19239=DIRECTION('center_axis',(0.,-1.,0.));
#19240=DIRECTION('ref_axis',(-1.,0.,0.));
#19241=DIRECTION('',(-1.,0.,0.));
#19242=DIRECTION('center_axis',(0.,-0.707106781186549,0.707106781186546));
#19243=DIRECTION('ref_axis',(1.,0.,0.));
#19244=DIRECTION('',(1.,0.,0.));
#19245=DIRECTION('center_axis',(0.,1.,0.));
#19246=DIRECTION('ref_axis',(1.,0.,0.));
#19247=DIRECTION('',(1.,0.,0.));
#19248=DIRECTION('center_axis',(0.,0.707106781186546,0.707106781186549));
#19249=DIRECTION('ref_axis',(1.,0.,0.));
#19250=DIRECTION('',(-1.,0.,0.));
#19251=DIRECTION('center_axis',(0.,-1.,0.));
#19252=DIRECTION('ref_axis',(-1.,0.,0.));
#19253=DIRECTION('',(-1.,0.,0.));
#19254=DIRECTION('center_axis',(0.,0.,-1.));
#19255=DIRECTION('ref_axis',(1.,0.,0.));
#19256=DIRECTION('',(0.707106781186548,-8.65956056235494E-17,0.707106781186547));
#19257=DIRECTION('center_axis',(0.,0.,1.));
#19258=DIRECTION('ref_axis',(1.,0.,0.));
#19259=DIRECTION('center_axis',(0.,0.,1.));
#19260=DIRECTION('ref_axis',(1.,0.,0.));
#19261=DIRECTION('',(0.,0.,1.));
#19262=DIRECTION('center_axis',(0.,0.,1.));
#19263=DIRECTION('ref_axis',(1.,0.,0.));
#19264=DIRECTION('center_axis',(0.,0.499999999999998,-0.86602540378444));
#19265=DIRECTION('ref_axis',(-1.,0.,0.));
#19266=DIRECTION('',(1.,0.,0.));
#19267=DIRECTION('',(-0.447213595499955,0.774596669241485,0.447213595499957));
#19268=DIRECTION('center_axis',(0.,0.866025403784439,-0.5));
#19269=DIRECTION('ref_axis',(0.,-0.5,-0.866025403784439));
#19270=DIRECTION('center_axis',(0.,0.866025403784439,-0.5));
#19271=DIRECTION('ref_axis',(0.,0.5,0.866025403784439));
#19272=DIRECTION('center_axis',(-0.707106781186549,0.,-0.707106781186546));
#19273=DIRECTION('ref_axis',(-0.707106781186546,0.,0.707106781186549));
#19274=DIRECTION('',(0.,1.,0.));
#19275=DIRECTION('center_axis',(-1.,0.,0.));
#19276=DIRECTION('ref_axis',(0.,0.,1.));
#19277=DIRECTION('center_axis',(0.,0.707106781186549,-0.707106781186546));
#19278=DIRECTION('ref_axis',(-1.,0.,0.));
#19279=DIRECTION('',(1.,0.,0.));
#19280=DIRECTION('center_axis',(0.,1.,0.));
#19281=DIRECTION('ref_axis',(1.,0.,0.));
#19282=DIRECTION('center_axis',(0.,-1.,0.));
#19283=DIRECTION('ref_axis',(1.,0.,0.));
#19284=DIRECTION('center_axis',(0.,3.41806786628767E-15,-1.));
#19285=DIRECTION('ref_axis',(1.,3.05029984904931E-17,0.));
#19286=DIRECTION('center_axis',(0.,0.,-1.));
#19287=DIRECTION('ref_axis',(1.,6.12323399573677E-17,0.));
#19288=DIRECTION('',(-0.382683432365089,3.09934474618468E-15,-0.923879532511287));
#19289=DIRECTION('center_axis',(0.,0.,1.));
#19290=DIRECTION('ref_axis',(1.,0.,0.));
#19291=DIRECTION('center_axis',(0.,0.,-1.));
#19292=DIRECTION('ref_axis',(1.,0.,0.));
#19293=DIRECTION('center_axis',(0.,0.,1.));
#19294=DIRECTION('ref_axis',(1.,6.12323399573677E-17,0.));
#19295=DIRECTION('',(-0.707106781186548,-8.65956056235493E-17,-0.707106781186548));
#19296=DIRECTION('center_axis',(0.,0.,1.));
#19297=DIRECTION('ref_axis',(1.,0.,0.));
#19298=DIRECTION('',(0.,0.,-1.));
#19299=DIRECTION('center_axis',(0.,0.,-1.));
#19300=DIRECTION('ref_axis',(1.,0.,0.));
#19301=DIRECTION('',(0.707106781186546,-8.65956056235491E-17,0.707106781186549));
#19302=DIRECTION('center_axis',(0.,0.,1.));
#19303=DIRECTION('ref_axis',(1.,0.,0.));
#19304=DIRECTION('center_axis',(0.,0.,-1.));
#19305=DIRECTION('ref_axis',(1.,0.,0.));
#19306=DIRECTION('center_axis',(0.,0.,-1.));
#19307=DIRECTION('ref_axis',(1.,0.,0.));
#19308=DIRECTION('',(0.,0.,-1.));
#19309=DIRECTION('center_axis',(0.,-8.23585751082044E-15,-1.));
#19310=DIRECTION('ref_axis',(1.,3.08934278087838E-17,0.));
#19311=DIRECTION('',(0.923879532511287,3.06712541512345E-15,0.38268343236509));
#19312=DIRECTION('center_axis',(0.,0.,-1.));
#19313=DIRECTION('ref_axis',(1.,0.,0.));
#19314=DIRECTION('center_axis',(0.,0.,1.));
#19315=DIRECTION('ref_axis',(1.,0.,0.));
#19316=DIRECTION('center_axis',(0.,0.,1.));
#19317=DIRECTION('ref_axis',(1.,0.,0.));
#19318=DIRECTION('center_axis',(0.,0.,-1.));
#19319=DIRECTION('ref_axis',(1.,0.,0.));
#19320=DIRECTION('center_axis',(0.,0.,-1.));
#19321=DIRECTION('ref_axis',(1.,0.,0.));
#19322=DIRECTION('center_axis',(0.,0.,1.));
#19323=DIRECTION('ref_axis',(1.,0.,0.));
#19324=DIRECTION('',(0.707106781186545,8.6595605623549E-17,-0.70710678118655));
#19325=DIRECTION('center_axis',(0.,-1.,0.));
#19326=DIRECTION('ref_axis',(1.,0.,0.));
#19327=DIRECTION('',(0.,-1.,0.));
#19328=DIRECTION('center_axis',(0.,-1.,0.));
#19329=DIRECTION('ref_axis',(1.,0.,0.));
#19330=DIRECTION('center_axis',(0.,1.,0.));
#19331=DIRECTION('ref_axis',(1.,0.,0.));
#19332=DIRECTION('center_axis',(0.,0.,1.));
#19333=DIRECTION('ref_axis',(1.,0.,0.));
#19334=DIRECTION('center_axis',(0.,0.,-1.));
#19335=DIRECTION('ref_axis',(1.,0.,0.));
#19336=DIRECTION('center_axis',(0.,0.,-1.));
#19337=DIRECTION('ref_axis',(1.,0.,0.));
#19338=DIRECTION('',(0.,0.,-1.));
#19339=DIRECTION('center_axis',(0.,0.,-1.));
#19340=DIRECTION('ref_axis',(1.,0.,0.));
#19341=DIRECTION('',(0.,0.,-1.));
#19342=DIRECTION('center_axis',(0.,0.,-1.));
#19343=DIRECTION('ref_axis',(1.,0.,0.));
#19344=DIRECTION('center_axis',(0.,0.,1.));
#19345=DIRECTION('ref_axis',(1.,0.,0.));
#19346=DIRECTION('center_axis',(0.,0.,-1.));
#19347=DIRECTION('ref_axis',(-1.,0.,0.));
#19348=DIRECTION('center_axis',(0.,0.,-1.));
#19349=DIRECTION('ref_axis',(-1.,0.,0.));
#19350=DIRECTION('center_axis',(0.,0.,-1.));
#19351=DIRECTION('ref_axis',(-1.,0.,0.));
#19352=DIRECTION('center_axis',(1.,0.,0.));
#19353=DIRECTION('ref_axis',(0.,-1.,0.));
#19354=DIRECTION('',(0.,0.,-1.));
#19355=DIRECTION('',(0.,-1.,0.));
#19356=DIRECTION('center_axis',(0.,1.,0.));
#19357=DIRECTION('ref_axis',(1.,0.,0.));
#19358=DIRECTION('',(1.,0.,0.));
#19359=DIRECTION('center_axis',(0.,0.,-1.));
#19360=DIRECTION('ref_axis',(-1.,0.,0.));
#19361=DIRECTION('axis',(0.,0.,1.));
#19362=DIRECTION('refdir',(1.,0.,0.));
#19363=DIRECTION('center_axis',(0.465479050687347,0.885058898249832,0.));
#19364=DIRECTION('ref_axis',(0.,0.,1.));
#19365=DIRECTION('',(0.,0.,1.));
#19366=DIRECTION('',(-0.885058898249832,0.465479050687346,0.));
#19367=DIRECTION('',(0.,0.,-1.));
#19368=DIRECTION('center_axis',(0.,0.,1.));
#19369=DIRECTION('ref_axis',(1.,0.,0.));
#19370=DIRECTION('center_axis',(0.,0.,-1.));
#19371=DIRECTION('ref_axis',(-1.,0.,0.));
#19372=DIRECTION('',(0.,0.,-1.));
#19373=DIRECTION('center_axis',(0.,0.,1.));
#19374=DIRECTION('ref_axis',(1.,0.,0.));
#19375=DIRECTION('center_axis',(0.,0.,1.));
#19376=DIRECTION('ref_axis',(-1.,0.,0.));
#19377=DIRECTION('center_axis',(0.,0.,1.));
#19378=DIRECTION('ref_axis',(-1.,0.,0.));
#19379=DIRECTION('center_axis',(-0.999538253627158,0.0303855152329365,0.));
#19380=DIRECTION('ref_axis',(0.,0.,1.));
#19381=DIRECTION('',(0.,0.,1.));
#19382=DIRECTION('',(-0.0303855152329365,-0.999538253627158,0.));
#19383=DIRECTION('',(0.,0.,-1.));
#19384=DIRECTION('center_axis',(0.,0.,1.));
#19385=DIRECTION('ref_axis',(1.,0.,0.));
#19386=DIRECTION('center_axis',(0.,0.,-1.));
#19387=DIRECTION('ref_axis',(-1.,0.,0.));
#19388=DIRECTION('',(0.,0.,-1.));
#19389=DIRECTION('center_axis',(0.,0.,1.));
#19390=DIRECTION('ref_axis',(1.,0.,0.));
#19391=DIRECTION('center_axis',(0.,0.,1.));
#19392=DIRECTION('ref_axis',(-1.,0.,0.));
#19393=DIRECTION('center_axis',(0.,0.,1.));
#19394=DIRECTION('ref_axis',(-1.,0.,0.));
#19395=DIRECTION('center_axis',(-0.473454498714793,-0.880818277311912,0.));
#19396=DIRECTION('ref_axis',(0.,0.,-1.));
#19397=DIRECTION('',(0.880818277311912,-0.473454498714793,0.));
#19398=DIRECTION('',(0.,0.,1.));
#19399=DIRECTION('center_axis',(0.,0.,1.));
#19400=DIRECTION('ref_axis',(0.848048096156423,0.529919264233209,0.));
#19401=DIRECTION('center_axis',(0.,0.,1.));
#19402=DIRECTION('ref_axis',(-0.848048096156426,-0.529919264233205,0.));
#19403=DIRECTION('',(0.,0.,-1.));
#19404=DIRECTION('center_axis',(0.,0.,1.));
#19405=DIRECTION('ref_axis',(-0.848048096156426,-0.529919264233205,0.));
#19406=DIRECTION('center_axis',(-0.994983842282394,0.100035761590367,0.));
#19407=DIRECTION('ref_axis',(0.,0.,1.));
#19408=DIRECTION('',(0.,0.,1.));
#19409=DIRECTION('',(-0.100035761590367,-0.994983842282394,0.));
#19410=DIRECTION('',(0.,0.,-1.));
#19411=DIRECTION('center_axis',(0.,0.,-1.));
#19412=DIRECTION('ref_axis',(0.913545457642601,0.4067366430758,0.));
#19413=DIRECTION('center_axis',(0.,0.,1.));
#19414=DIRECTION('ref_axis',(0.913545457642601,0.4067366430758,0.));
#19415=DIRECTION('center_axis',(0.,0.,-1.));
#19416=DIRECTION('ref_axis',(0.913545457642601,0.4067366430758,0.));
#19417=DIRECTION('center_axis',(0.,0.,1.));
#19418=DIRECTION('ref_axis',(0.913545457642598,0.406736643075806,0.));
#19419=DIRECTION('center_axis',(0.,0.,1.));
#19420=DIRECTION('ref_axis',(-0.913545457642601,-0.4067366430758,0.));
#19421=DIRECTION('',(0.,0.,1.));
#19422=DIRECTION('center_axis',(-0.533743964386135,-0.845646131949631,0.));
#19423=DIRECTION('ref_axis',(0.,0.,1.));
#19424=DIRECTION('',(0.84564613194963,-0.533743964386135,0.));
#19425=DIRECTION('',(0.,0.,-1.));
#19426=DIRECTION('',(0.,0.,1.));
#19427=DIRECTION('center_axis',(0.,0.,1.));
#19428=DIRECTION('ref_axis',(0.882947592858955,0.469471562785839,0.));
#19429=DIRECTION('center_axis',(0.,0.,1.));
#19430=DIRECTION('ref_axis',(-0.882947592858927,-0.469471562785891,0.));
#19431=DIRECTION('center_axis',(0.,0.,1.));
#19432=DIRECTION('ref_axis',(0.882947592858927,0.469471562785891,0.));
#19433=DIRECTION('center_axis',(0.,0.,-1.));
#19434=DIRECTION('ref_axis',(0.882947592858927,0.469471562785891,0.));
#19435=DIRECTION('center_axis',(0.,0.,-1.));
#19436=DIRECTION('ref_axis',(0.882947592858927,0.469471562785891,0.));
#19437=DIRECTION('center_axis',(-0.985581969673453,0.169198643772926,0.));
#19438=DIRECTION('ref_axis',(0.,0.,1.));
#19439=DIRECTION('',(0.,0.,1.));
#19440=DIRECTION('',(-0.169198643772926,-0.985581969673453,0.));
#19441=DIRECTION('',(0.,0.,-1.));
#19442=DIRECTION('center_axis',(0.,0.,-1.));
#19443=DIRECTION('ref_axis',(0.939692620785908,0.342020143325669,0.));
#19444=DIRECTION('center_axis',(0.,0.,1.));
#19445=DIRECTION('ref_axis',(0.939692620785908,0.342020143325669,0.));
#19446=DIRECTION('center_axis',(0.,0.,-1.));
#19447=DIRECTION('ref_axis',(0.939692620785908,0.342020143325669,0.));
#19448=DIRECTION('center_axis',(0.,0.,1.));
#19449=DIRECTION('ref_axis',(0.939692620785908,0.342020143325671,0.));
#19450=DIRECTION('center_axis',(0.,0.,1.));
#19451=DIRECTION('ref_axis',(-0.939692620785908,-0.342020143325669,0.));
#19452=DIRECTION('',(0.,0.,1.));
#19453=DIRECTION('center_axis',(-0.591433083115112,-0.80635408363631,0.));
#19454=DIRECTION('ref_axis',(0.,0.,1.));
#19455=DIRECTION('',(0.80635408363631,-0.591433083115112,0.));
#19456=DIRECTION('',(0.,0.,-1.));
#19457=DIRECTION('center_axis',(-0.646240799313603,-0.763133559282066,0.));
#19458=DIRECTION('ref_axis',(0.,0.,1.));
#19459=DIRECTION('',(0.763133559282066,-0.646240799313603,0.));
#19460=DIRECTION('',(0.,0.,-1.));
#19461=DIRECTION('center_axis',(-0.928866262851607,-0.370415261208404,0.));
#19462=DIRECTION('ref_axis',(0.,0.,1.));
#19463=DIRECTION('',(0.370415261208404,-0.928866262851607,0.));
#19464=DIRECTION('',(0.,0.,-1.));
#19465=DIRECTION('',(0.,0.,1.));
#19466=DIRECTION('center_axis',(0.,0.,1.));
#19467=DIRECTION('ref_axis',(0.990268068741571,-0.139173100960063,0.));
#19468=DIRECTION('center_axis',(0.,0.,1.));
#19469=DIRECTION('ref_axis',(-0.99026806874157,0.139173100960065,0.));
#19470=DIRECTION('',(0.,0.,-1.));
#19471=DIRECTION('center_axis',(0.,0.,1.));
#19472=DIRECTION('ref_axis',(-0.99026806874157,0.139173100960065,0.));
#19473=DIRECTION('center_axis',(0.,0.,1.));
#19474=DIRECTION('ref_axis',(-1.,0.,0.));
#19475=DIRECTION('center_axis',(0.,0.,-1.));
#19476=DIRECTION('ref_axis',(-1.,0.,0.));
#19477=DIRECTION('center_axis',(0.,0.,1.));
#19478=DIRECTION('ref_axis',(-1.,0.,0.));
#19479=DIRECTION('center_axis',(-0.697900095297593,0.71619512493706,0.));
#19480=DIRECTION('ref_axis',(0.,0.,1.));
#19481=DIRECTION('',(0.,0.,1.));
#19482=DIRECTION('',(-0.71619512493706,-0.697900095297593,0.));
#19483=DIRECTION('',(0.,0.,-1.));
#19484=DIRECTION('center_axis',(0.,0.,1.));
#19485=DIRECTION('ref_axis',(1.,0.,0.));
#19486=DIRECTION('center_axis',(0.,0.,-1.));
#19487=DIRECTION('ref_axis',(-1.,0.,0.));
#19488=DIRECTION('',(0.,0.,-1.));
#19489=DIRECTION('center_axis',(0.,0.,1.));
#19490=DIRECTION('ref_axis',(1.,0.,0.));
#19491=DIRECTION('center_axis',(0.,0.,1.));
#19492=DIRECTION('ref_axis',(-1.,0.,0.));
#19493=DIRECTION('center_axis',(0.,0.,1.));
#19494=DIRECTION('ref_axis',(-1.,0.,0.));
#19495=DIRECTION('center_axis',(-0.971378440778567,-0.237537207171004,0.));
#19496=DIRECTION('ref_axis',(0.,0.,1.));
#19497=DIRECTION('',(0.237537207171004,-0.971378440778567,0.));
#19498=DIRECTION('',(0.,0.,-1.));
#19499=DIRECTION('',(0.,0.,1.));
#19500=DIRECTION('center_axis',(0.,0.,1.));
#19501=DIRECTION('ref_axis',(-1.,0.,0.));
#19502=DIRECTION('center_axis',(0.,0.,-1.));
#19503=DIRECTION('ref_axis',(-1.,0.,0.));
#19504=DIRECTION('center_axis',(0.,0.,1.));
#19505=DIRECTION('ref_axis',(-1.,0.,0.));
#19506=DIRECTION('center_axis',(0.,0.,1.));
#19507=DIRECTION('ref_axis',(1.,0.,0.));
#19508=DIRECTION('center_axis',(0.,0.,1.));
#19509=DIRECTION('ref_axis',(1.,0.,0.));
#19510=DIRECTION('',(0.,0.,1.));
#19511=DIRECTION('center_axis',(-0.646240799313457,0.763133559282191,0.));
#19512=DIRECTION('ref_axis',(0.,0.,1.));
#19513=DIRECTION('',(-0.763133559282191,-0.646240799313457,0.));
#19514=DIRECTION('',(0.,0.,-1.));
#19515=DIRECTION('center_axis',(-0.985581969673418,-0.169198643773126,0.));
#19516=DIRECTION('ref_axis',(0.,0.,1.));
#19517=DIRECTION('',(0.169198643773126,-0.985581969673418,0.));
#19518=DIRECTION('',(0.,0.,-1.));
#19519=DIRECTION('',(0.,0.,1.));
#19520=DIRECTION('center_axis',(0.,0.,1.));
#19521=DIRECTION('ref_axis',(-1.,0.,0.));
#19522=DIRECTION('center_axis',(0.,0.,-1.));
#19523=DIRECTION('ref_axis',(-1.,0.,0.));
#19524=DIRECTION('center_axis',(0.,0.,1.));
#19525=DIRECTION('ref_axis',(-1.,0.,0.));
#19526=DIRECTION('center_axis',(0.,0.,1.));
#19527=DIRECTION('ref_axis',(1.,0.,0.));
#19528=DIRECTION('center_axis',(0.,0.,1.));
#19529=DIRECTION('ref_axis',(1.,0.,0.));
#19530=DIRECTION('',(0.,0.,1.));
#19531=DIRECTION('center_axis',(-0.591433083115099,0.806354083636319,0.));
#19532=DIRECTION('ref_axis',(0.,0.,1.));
#19533=DIRECTION('',(-0.806354083636319,-0.591433083115099,0.));
#19534=DIRECTION('',(0.,0.,-1.));
#19535=DIRECTION('center_axis',(-0.994983842282392,-0.100035761590388,0.));
#19536=DIRECTION('ref_axis',(0.,0.,1.));
#19537=DIRECTION('',(0.100035761590388,-0.994983842282392,0.));
#19538=DIRECTION('',(0.,0.,-1.));
#19539=DIRECTION('',(0.,0.,1.));
#19540=DIRECTION('center_axis',(0.,0.,1.));
#19541=DIRECTION('ref_axis',(-1.,0.,0.));
#19542=DIRECTION('center_axis',(0.,0.,-1.));
#19543=DIRECTION('ref_axis',(-1.,0.,0.));
#19544=DIRECTION('center_axis',(0.,0.,1.));
#19545=DIRECTION('ref_axis',(-1.,0.,0.));
#19546=DIRECTION('center_axis',(0.,0.,1.));
#19547=DIRECTION('ref_axis',(1.,0.,0.));
#19548=DIRECTION('center_axis',(0.,0.,1.));
#19549=DIRECTION('ref_axis',(1.,0.,0.));
#19550=DIRECTION('',(0.,0.,1.));
#19551=DIRECTION('center_axis',(-0.533743964386147,0.845646131949623,0.));
#19552=DIRECTION('ref_axis',(0.,0.,1.));
#19553=DIRECTION('',(-0.845646131949623,-0.533743964386147,0.));
#19554=DIRECTION('',(0.,0.,-1.));
#19555=DIRECTION('center_axis',(-0.999538253627158,-0.0303855152329365,
0.));
#19556=DIRECTION('ref_axis',(0.,0.,1.));
#19557=DIRECTION('',(0.0303855152329365,-0.999538253627158,0.));
#19558=DIRECTION('',(0.,0.,-1.));
#19559=DIRECTION('',(0.,0.,1.));
#19560=DIRECTION('center_axis',(0.,0.,1.));
#19561=DIRECTION('ref_axis',(-1.,0.,0.));
#19562=DIRECTION('center_axis',(0.,0.,-1.));
#19563=DIRECTION('ref_axis',(-1.,0.,0.));
#19564=DIRECTION('center_axis',(0.,0.,1.));
#19565=DIRECTION('ref_axis',(-1.,0.,0.));
#19566=DIRECTION('center_axis',(0.,0.,1.));
#19567=DIRECTION('ref_axis',(1.,0.,0.));
#19568=DIRECTION('center_axis',(0.,0.,1.));
#19569=DIRECTION('ref_axis',(1.,0.,0.));
#19570=DIRECTION('',(0.,0.,1.));
#19571=DIRECTION('center_axis',(-0.473454498714793,0.880818277311912,0.));
#19572=DIRECTION('ref_axis',(0.,0.,1.));
#19573=DIRECTION('',(-0.880818277311912,-0.473454498714793,0.));
#19574=DIRECTION('',(0.,0.,-1.));
#19575=DIRECTION('center_axis',(-0.999223015073487,0.0394127663004103,0.));
#19576=DIRECTION('ref_axis',(0.,0.,1.));
#19577=DIRECTION('',(-0.0394127663004103,-0.999223015073487,0.));
#19578=DIRECTION('',(0.,0.,-1.));
#19579=DIRECTION('',(0.,0.,1.));
#19580=DIRECTION('center_axis',(0.,0.,1.));
#19581=DIRECTION('ref_axis',(-1.,0.,0.));
#19582=DIRECTION('center_axis',(0.,0.,-1.));
#19583=DIRECTION('ref_axis',(-1.,0.,0.));
#19584=DIRECTION('center_axis',(0.,0.,1.));
#19585=DIRECTION('ref_axis',(-1.,0.,0.));
#19586=DIRECTION('center_axis',(0.,0.,1.));
#19587=DIRECTION('ref_axis',(1.,0.,0.));
#19588=DIRECTION('center_axis',(0.,0.,1.));
#19589=DIRECTION('ref_axis',(1.,0.,0.));
#19590=DIRECTION('',(0.,0.,1.));
#19591=DIRECTION('center_axis',(-0.410858410316824,0.911699164566872,0.));
#19592=DIRECTION('ref_axis',(0.,0.,1.));
#19593=DIRECTION('',(-0.911699164566872,-0.410858410316824,0.));
#19594=DIRECTION('',(0.,0.,-1.));
#19595=DIRECTION('center_axis',(-0.994039662431944,0.109019032797885,0.));
#19596=DIRECTION('ref_axis',(0.,0.,1.));
#19597=DIRECTION('',(-0.109019032797885,-0.994039662431944,0.));
#19598=DIRECTION('',(0.,0.,-1.));
#19599=DIRECTION('',(0.,0.,1.));
#19600=DIRECTION('center_axis',(0.,0.,1.));
#19601=DIRECTION('ref_axis',(-1.,0.,0.));
#19602=DIRECTION('center_axis',(0.,0.,-1.));
#19603=DIRECTION('ref_axis',(-1.,0.,0.));
#19604=DIRECTION('center_axis',(0.,0.,1.));
#19605=DIRECTION('ref_axis',(-1.,0.,0.));
#19606=DIRECTION('center_axis',(0.,0.,1.));
#19607=DIRECTION('ref_axis',(1.,0.,0.));
#19608=DIRECTION('center_axis',(0.,0.,1.));
#19609=DIRECTION('ref_axis',(1.,0.,0.));
#19610=DIRECTION('',(0.,0.,1.));
#19611=DIRECTION('center_axis',(-0.346260661043308,0.938138345135648,0.));
#19612=DIRECTION('ref_axis',(0.,0.,1.));
#19613=DIRECTION('',(-0.938138345135648,-0.346260661043308,0.));
#19614=DIRECTION('',(0.,0.,-1.));
#19615=DIRECTION('center_axis',(-0.984013448475546,0.178094169526304,0.));
#19616=DIRECTION('ref_axis',(0.,0.,1.));
#19617=DIRECTION('',(-0.178094169526304,-0.984013448475546,0.));
#19618=DIRECTION('',(0.,0.,-1.));
#19619=DIRECTION('',(0.,0.,1.));
#19620=DIRECTION('center_axis',(0.,0.,1.));
#19621=DIRECTION('ref_axis',(-1.,0.,0.));
#19622=DIRECTION('center_axis',(0.,0.,-1.));
#19623=DIRECTION('ref_axis',(-1.,0.,0.));
#19624=DIRECTION('center_axis',(0.,0.,1.));
#19625=DIRECTION('ref_axis',(-1.,0.,0.));
#19626=DIRECTION('center_axis',(0.,0.,1.));
#19627=DIRECTION('ref_axis',(1.,0.,0.));
#19628=DIRECTION('center_axis',(0.,0.,1.));
#19629=DIRECTION('ref_axis',(1.,0.,0.));
#19630=DIRECTION('',(0.,0.,1.));
#19631=DIRECTION('center_axis',(-0.279975964635197,0.960007009988256,0.));
#19632=DIRECTION('ref_axis',(0.,0.,1.));
#19633=DIRECTION('',(-0.960007009988256,-0.279975964635197,0.));
#19634=DIRECTION('',(0.,0.,-1.));
#19635=DIRECTION('center_axis',(-0.969193219910809,0.246301649362969,0.));
#19636=DIRECTION('ref_axis',(0.,0.,1.));
#19637=DIRECTION('',(-0.246301649362969,-0.969193219910809,0.));
#19638=DIRECTION('',(0.,0.,-1.));
#19639=DIRECTION('',(0.,0.,1.));
#19640=DIRECTION('center_axis',(0.,0.,1.));
#19641=DIRECTION('ref_axis',(-1.,0.,0.));
#19642=DIRECTION('center_axis',(0.,0.,-1.));
#19643=DIRECTION('ref_axis',(-1.,0.,0.));
#19644=DIRECTION('center_axis',(0.,0.,1.));
#19645=DIRECTION('ref_axis',(-1.,0.,0.));
#19646=DIRECTION('center_axis',(0.,0.,1.));
#19647=DIRECTION('ref_axis',(1.,0.,0.));
#19648=DIRECTION('center_axis',(0.,0.,1.));
#19649=DIRECTION('ref_axis',(1.,0.,0.));
#19650=DIRECTION('',(0.,0.,1.));
#19651=DIRECTION('center_axis',(-0.212327253470465,0.977198617187769,0.));
#19652=DIRECTION('ref_axis',(0.,0.,1.));
#19653=DIRECTION('',(-0.977198617187769,-0.212327253470465,0.));
#19654=DIRECTION('',(0.,0.,-1.));
#19655=DIRECTION('center_axis',(0.,0.,-1.));
#19656=DIRECTION('ref_axis',(0.669130606358858,-0.743144825477394,0.));
#19657=DIRECTION('center_axis',(0.,0.,1.));
#19658=DIRECTION('ref_axis',(0.669130606358858,-0.743144825477394,0.));
#19659=DIRECTION('center_axis',(0.,0.,-1.));
#19660=DIRECTION('ref_axis',(0.669130606358858,-0.743144825477394,0.));
#19661=DIRECTION('center_axis',(0.,0.,1.));
#19662=DIRECTION('ref_axis',(-1.,0.,0.));
#19663=DIRECTION('center_axis',(0.,0.,1.));
#19664=DIRECTION('ref_axis',(-1.,0.,0.));
#19665=DIRECTION('center_axis',(0.,0.,-1.));
#19666=DIRECTION('ref_axis',(-1.,0.,0.));
#19667=DIRECTION('center_axis',(0.,0.,1.));
#19668=DIRECTION('ref_axis',(-1.,0.,0.));
#19669=DIRECTION('center_axis',(0.,0.,1.));
#19670=DIRECTION('ref_axis',(-1.,0.,0.));
#19671=DIRECTION('center_axis',(0.,0.,-1.));
#19672=DIRECTION('ref_axis',(-1.,0.,0.));
#19673=DIRECTION('center_axis',(0.,0.,1.));
#19674=DIRECTION('ref_axis',(-1.,0.,0.));
#19675=DIRECTION('center_axis',(0.,0.,-1.));
#19676=DIRECTION('ref_axis',(-1.,0.,0.));
#19677=DIRECTION('center_axis',(0.,0.,1.));
#19678=DIRECTION('ref_axis',(-1.,0.,0.));
#19679=DIRECTION('center_axis',(0.,0.,1.));
#19680=DIRECTION('ref_axis',(1.,0.,0.));
#19681=DIRECTION('center_axis',(0.,0.,1.));
#19682=DIRECTION('ref_axis',(-0.961261695938319,-0.275637355816999,0.));
#19683=DIRECTION('center_axis',(0.,0.,1.));
#19684=DIRECTION('ref_axis',(-1.,0.,0.));
#19685=DIRECTION('center_axis',(0.,0.,1.));
#19686=DIRECTION('ref_axis',(-0.978147600733806,-0.20791169081776,0.));
#19687=DIRECTION('center_axis',(0.,0.,1.));
#19688=DIRECTION('ref_axis',(-1.,0.,0.));
#19689=DIRECTION('center_axis',(0.,0.,1.));
#19690=DIRECTION('ref_axis',(-0.99026806874157,-0.139173100960066,0.));
#19691=DIRECTION('center_axis',(0.,0.,1.));
#19692=DIRECTION('ref_axis',(-1.,0.,0.));
#19693=DIRECTION('center_axis',(0.,0.,1.));
#19694=DIRECTION('ref_axis',(-0.997564050259824,-0.0697564737441253,0.));
#19695=DIRECTION('center_axis',(0.,0.,1.));
#19696=DIRECTION('ref_axis',(-1.,0.,0.));
#19697=DIRECTION('center_axis',(0.,0.,1.));
#19698=DIRECTION('ref_axis',(-1.,1.22464679914735E-16,0.));
#19699=DIRECTION('center_axis',(0.,0.,1.));
#19700=DIRECTION('ref_axis',(-1.,0.,0.));
#19701=DIRECTION('center_axis',(0.,0.,1.));
#19702=DIRECTION('ref_axis',(-0.997564050259824,0.0697564737441255,0.));
#19703=DIRECTION('center_axis',(0.,0.,1.));
#19704=DIRECTION('ref_axis',(-1.,0.,0.));
#19705=DIRECTION('center_axis',(0.,0.,1.));
#19706=DIRECTION('ref_axis',(-0.978147600733806,0.207911690817759,0.));
#19707=DIRECTION('center_axis',(0.,0.,-1.));
#19708=DIRECTION('ref_axis',(0.961261695938319,-0.275637355816999,0.));
#19709=DIRECTION('center_axis',(0.,0.,-1.));
#19710=DIRECTION('ref_axis',(0.939692620785908,-0.342020143325669,0.));
#19711=DIRECTION('center_axis',(0.,0.,-1.));
#19712=DIRECTION('ref_axis',(0.913545457642601,-0.4067366430758,0.));
#19713=DIRECTION('center_axis',(0.,0.,-1.));
#19714=DIRECTION('ref_axis',(0.882947592858927,-0.469471562785891,0.));
#19715=DIRECTION('center_axis',(0.,0.,-1.));
#19716=DIRECTION('ref_axis',(0.848048096156426,-0.529919264233205,0.));
#19717=DIRECTION('center_axis',(0.,0.,-1.));
#19718=DIRECTION('ref_axis',(0.809016994374947,-0.587785252292473,0.));
#19719=DIRECTION('center_axis',(0.,0.,-1.));
#19720=DIRECTION('ref_axis',(0.766044443118978,-0.642787609686539,0.));
#19721=DIRECTION('center_axis',(0.,0.,-1.));
#19722=DIRECTION('ref_axis',(0.719339800338651,-0.694658370458997,0.));
#19723=DIRECTION('center_axis',(0.,0.,1.));
#19724=DIRECTION('ref_axis',(-1.,0.,0.));
#19725=DIRECTION('center_axis',(0.,0.,-1.));
#19726=DIRECTION('ref_axis',(0.615661475325658,-0.788010753606722,0.));
#19727=DIRECTION('center_axis',(0.,0.,1.));
#19728=DIRECTION('ref_axis',(-1.,0.,0.));
#19729=DIRECTION('center_axis',(0.,0.,-1.));
#19730=DIRECTION('ref_axis',(0.559192903470747,-0.829037572555042,0.));
#19731=DIRECTION('center_axis',(0.,0.,1.));
#19732=DIRECTION('ref_axis',(-1.,0.,0.));
#19733=DIRECTION('center_axis',(0.,0.,-1.));
#19734=DIRECTION('ref_axis',(0.5,-0.866025403784439,0.));
#19735=DIRECTION('center_axis',(0.,0.,1.));
#19736=DIRECTION('ref_axis',(-1.,0.,0.));
#19737=DIRECTION('center_axis',(0.,0.,-1.));
#19738=DIRECTION('ref_axis',(0.438371146789078,-0.898794046299167,0.));
#19739=DIRECTION('center_axis',(0.,0.,1.));
#19740=DIRECTION('ref_axis',(-1.,0.,0.));
#19741=DIRECTION('center_axis',(0.,0.,-1.));
#19742=DIRECTION('ref_axis',(0.374606593415912,-0.927183854566787,0.));
#19743=DIRECTION('center_axis',(0.,0.,1.));
#19744=DIRECTION('ref_axis',(-1.,0.,0.));
#19745=DIRECTION('center_axis',(0.,0.,-1.));
#19746=DIRECTION('ref_axis',(0.309016994374947,-0.951056516295154,0.));
#19747=DIRECTION('center_axis',(0.,0.,1.));
#19748=DIRECTION('ref_axis',(-1.,0.,0.));
#19749=DIRECTION('center_axis',(0.,0.,-1.));
#19750=DIRECTION('ref_axis',(0.241921895599668,-0.970295726275997,0.));
#19751=DIRECTION('center_axis',(0.,0.,1.));
#19752=DIRECTION('ref_axis',(-1.,0.,0.));
#19753=DIRECTION('center_axis',(0.,0.,-1.));
#19754=DIRECTION('ref_axis',(0.17364817766693,-0.984807753012208,0.));
#19755=DIRECTION('center_axis',(0.,0.,1.));
#19756=DIRECTION('ref_axis',(-1.,0.,0.));
#19757=DIRECTION('center_axis',(0.,0.,-1.));
#19758=DIRECTION('ref_axis',(0.104528463267654,-0.994521895368273,0.));
#19759=DIRECTION('center_axis',(0.,0.,1.));
#19760=DIRECTION('ref_axis',(-0.034899496702501,0.999390827019096,0.));
#19761=DIRECTION('center_axis',(0.,0.,1.));
#19762=DIRECTION('ref_axis',(1.,0.,0.));
#19763=DIRECTION('center_axis',(0.,0.,1.));
#19764=DIRECTION('ref_axis',(0.0348994967025011,0.999390827019096,0.));
#19765=DIRECTION('center_axis',(0.,0.,1.));
#19766=DIRECTION('ref_axis',(1.,0.,0.));
#19767=DIRECTION('center_axis',(0.,0.,-1.));
#19768=DIRECTION('ref_axis',(-0.104528463267653,-0.994521895368273,0.));
#19769=DIRECTION('center_axis',(0.,0.,1.));
#19770=DIRECTION('ref_axis',(1.,0.,0.));
#19771=DIRECTION('center_axis',(0.,0.,-1.));
#19772=DIRECTION('ref_axis',(-0.17364817766693,-0.984807753012208,0.));
#19773=DIRECTION('center_axis',(0.,0.,1.));
#19774=DIRECTION('ref_axis',(1.,0.,0.));
#19775=DIRECTION('center_axis',(0.,0.,-1.));
#19776=DIRECTION('ref_axis',(-0.241921895599668,-0.970295726275997,0.));
#19777=DIRECTION('center_axis',(0.,0.,1.));
#19778=DIRECTION('ref_axis',(1.,0.,0.));
#19779=DIRECTION('center_axis',(0.,0.,-1.));
#19780=DIRECTION('ref_axis',(-0.309016994374947,-0.951056516295154,0.));
#19781=DIRECTION('center_axis',(0.,0.,1.));
#19782=DIRECTION('ref_axis',(1.,0.,0.));
#19783=DIRECTION('center_axis',(0.,0.,-1.));
#19784=DIRECTION('ref_axis',(-0.374606593415912,-0.927183854566787,0.));
#19785=DIRECTION('center_axis',(0.,0.,1.));
#19786=DIRECTION('ref_axis',(1.,0.,0.));
#19787=DIRECTION('center_axis',(0.,0.,-1.));
#19788=DIRECTION('ref_axis',(-0.438371146789078,-0.898794046299167,0.));
#19789=DIRECTION('center_axis',(0.,0.,1.));
#19790=DIRECTION('ref_axis',(1.,0.,0.));
#19791=DIRECTION('center_axis',(0.,0.,-1.));
#19792=DIRECTION('ref_axis',(-0.5,-0.866025403784439,0.));
#19793=DIRECTION('center_axis',(0.,0.,1.));
#19794=DIRECTION('ref_axis',(1.,0.,0.));
#19795=DIRECTION('center_axis',(0.,0.,-1.));
#19796=DIRECTION('ref_axis',(-0.559192903470747,-0.829037572555042,0.));
#19797=DIRECTION('center_axis',(0.,0.,1.));
#19798=DIRECTION('ref_axis',(1.,0.,0.));
#19799=DIRECTION('center_axis',(0.,0.,1.));
#19800=DIRECTION('ref_axis',(0.615661475325658,0.788010753606722,0.));
#19801=DIRECTION('center_axis',(0.,0.,1.));
#19802=DIRECTION('ref_axis',(1.,0.,0.));
#19803=DIRECTION('center_axis',(0.,0.,-1.));
#19804=DIRECTION('ref_axis',(-0.669130606358858,-0.743144825477394,0.));
#19805=DIRECTION('center_axis',(0.,0.,1.));
#19806=DIRECTION('ref_axis',(1.,0.,0.));
#19807=DIRECTION('center_axis',(0.,0.,1.));
#19808=DIRECTION('ref_axis',(0.719339800338651,0.694658370458997,0.));
#19809=DIRECTION('center_axis',(0.,0.,1.));
#19810=DIRECTION('ref_axis',(1.,0.,0.));
#19811=DIRECTION('center_axis',(0.,0.,-1.));
#19812=DIRECTION('ref_axis',(-0.766044443118978,-0.642787609686539,0.));
#19813=DIRECTION('center_axis',(0.,0.,1.));
#19814=DIRECTION('ref_axis',(1.,0.,0.));
#19815=DIRECTION('center_axis',(0.,0.,-1.));
#19816=DIRECTION('ref_axis',(-0.809016994374947,-0.587785252292473,0.));
#19817=DIRECTION('center_axis',(0.,0.,1.));
#19818=DIRECTION('ref_axis',(1.,0.,0.));
#19819=DIRECTION('center_axis',(0.,0.,-1.));
#19820=DIRECTION('ref_axis',(-0.848048096156426,-0.529919264233205,0.));
#19821=DIRECTION('center_axis',(0.,0.,1.));
#19822=DIRECTION('ref_axis',(1.,0.,0.));
#19823=DIRECTION('center_axis',(0.,0.,-1.));
#19824=DIRECTION('ref_axis',(-0.882947592858927,-0.469471562785891,0.));
#19825=DIRECTION('center_axis',(0.,0.,1.));
#19826=DIRECTION('ref_axis',(1.,0.,0.));
#19827=DIRECTION('center_axis',(0.,0.,-1.));
#19828=DIRECTION('ref_axis',(-0.913545457642601,-0.4067366430758,0.));
#19829=DIRECTION('center_axis',(0.,0.,1.));
#19830=DIRECTION('ref_axis',(1.,0.,0.));
#19831=DIRECTION('center_axis',(0.,0.,-1.));
#19832=DIRECTION('ref_axis',(-0.939692620785908,-0.342020143325669,0.));
#19833=DIRECTION('center_axis',(0.,0.,1.));
#19834=DIRECTION('ref_axis',(1.,0.,0.));
#19835=DIRECTION('center_axis',(0.,0.,-1.));
#19836=DIRECTION('ref_axis',(-0.961261695938319,-0.275637355816999,0.));
#19837=DIRECTION('center_axis',(0.,0.,1.));
#19838=DIRECTION('ref_axis',(1.,0.,0.));
#19839=DIRECTION('center_axis',(0.,0.,1.));
#19840=DIRECTION('ref_axis',(0.978147600733806,0.207911690817759,0.));
#19841=DIRECTION('center_axis',(0.,0.,1.));
#19842=DIRECTION('ref_axis',(1.,0.,0.));
#19843=DIRECTION('center_axis',(0.,0.,-1.));
#19844=DIRECTION('ref_axis',(-0.99026806874157,-0.139173100960065,0.));
#19845=DIRECTION('center_axis',(0.,0.,1.));
#19846=DIRECTION('ref_axis',(1.,0.,0.));
#19847=DIRECTION('center_axis',(0.,0.,-1.));
#19848=DIRECTION('ref_axis',(-0.997564050259824,-0.0697564737441253,0.));
#19849=DIRECTION('center_axis',(0.,0.,1.));
#19850=DIRECTION('ref_axis',(1.,0.,0.));
#19851=DIRECTION('center_axis',(0.,0.,1.));
#19852=DIRECTION('ref_axis',(1.,0.,0.));
#19853=DIRECTION('center_axis',(0.,0.,1.));
#19854=DIRECTION('ref_axis',(1.,0.,0.));
#19855=DIRECTION('center_axis',(0.,0.,-1.));
#19856=DIRECTION('ref_axis',(-0.997564050259824,0.0697564737441256,0.));
#19857=DIRECTION('center_axis',(0.,0.,1.));
#19858=DIRECTION('ref_axis',(1.,0.,0.));
#19859=DIRECTION('center_axis',(0.,0.,-1.));
#19860=DIRECTION('ref_axis',(-0.99026806874157,0.139173100960066,0.));
#19861=DIRECTION('center_axis',(0.,0.,1.));
#19862=DIRECTION('ref_axis',(1.,0.,0.));
#19863=DIRECTION('center_axis',(0.,0.,-1.));
#19864=DIRECTION('ref_axis',(-0.978147600733805,0.20791169081776,0.));
#19865=DIRECTION('center_axis',(0.,0.,1.));
#19866=DIRECTION('ref_axis',(1.,0.,0.));
#19867=DIRECTION('center_axis',(0.,0.,-1.));
#19868=DIRECTION('ref_axis',(-0.961261695938319,0.275637355816999,0.));
#19869=DIRECTION('center_axis',(0.,0.,1.));
#19870=DIRECTION('ref_axis',(1.,0.,0.));
#19871=DIRECTION('center_axis',(0.,0.,-1.));
#19872=DIRECTION('ref_axis',(-0.939692620785908,0.342020143325669,0.));
#19873=DIRECTION('center_axis',(0.,0.,1.));
#19874=DIRECTION('ref_axis',(1.,0.,0.));
#19875=DIRECTION('center_axis',(0.,0.,-1.));
#19876=DIRECTION('ref_axis',(-0.913545457642601,0.4067366430758,0.));
#19877=DIRECTION('center_axis',(0.,0.,1.));
#19878=DIRECTION('ref_axis',(1.,0.,0.));
#19879=DIRECTION('center_axis',(0.,0.,1.));
#19880=DIRECTION('ref_axis',(0.882947592858927,-0.469471562785891,0.));
#19881=DIRECTION('center_axis',(0.,0.,1.));
#19882=DIRECTION('ref_axis',(1.,0.,0.));
#19883=DIRECTION('center_axis',(0.,0.,-1.));
#19884=DIRECTION('ref_axis',(-0.848048096156426,0.529919264233205,0.));
#19885=DIRECTION('center_axis',(0.,0.,1.));
#19886=DIRECTION('ref_axis',(1.,0.,0.));
#19887=DIRECTION('center_axis',(0.,0.,-1.));
#19888=DIRECTION('ref_axis',(-0.809016994374947,0.587785252292473,0.));
#19889=DIRECTION('center_axis',(0.,0.,1.));
#19890=DIRECTION('ref_axis',(1.,0.,0.));
#19891=DIRECTION('center_axis',(0.,0.,-1.));
#19892=DIRECTION('ref_axis',(-0.766044443118978,0.64278760968654,0.));
#19893=DIRECTION('center_axis',(0.,0.,1.));
#19894=DIRECTION('ref_axis',(1.,0.,0.));
#19895=DIRECTION('center_axis',(0.,0.,1.));
#19896=DIRECTION('ref_axis',(0.719339800338651,-0.694658370458998,0.));
#19897=DIRECTION('center_axis',(0.,0.,1.));
#19898=DIRECTION('ref_axis',(1.,0.,0.));
#19899=DIRECTION('center_axis',(0.,0.,-1.));
#19900=DIRECTION('ref_axis',(-0.669130606358858,0.743144825477395,0.));
#19901=DIRECTION('center_axis',(0.,0.,1.));
#19902=DIRECTION('ref_axis',(1.,0.,0.));
#19903=DIRECTION('center_axis',(0.,0.,-1.));
#19904=DIRECTION('ref_axis',(-0.615661475325659,0.788010753606722,0.));
#19905=DIRECTION('center_axis',(0.,0.,1.));
#19906=DIRECTION('ref_axis',(1.,0.,0.));
#19907=DIRECTION('center_axis',(0.,0.,-1.));
#19908=DIRECTION('ref_axis',(-0.559192903470747,0.829037572555042,0.));
#19909=DIRECTION('center_axis',(0.,0.,1.));
#19910=DIRECTION('ref_axis',(1.,0.,0.));
#19911=DIRECTION('center_axis',(0.,0.,-1.));
#19912=DIRECTION('ref_axis',(-0.5,0.866025403784439,0.));
#19913=DIRECTION('center_axis',(0.,0.,1.));
#19914=DIRECTION('ref_axis',(1.,0.,0.));
#19915=DIRECTION('center_axis',(0.,0.,-1.));
#19916=DIRECTION('ref_axis',(-0.438371146789077,0.898794046299167,0.));
#19917=DIRECTION('center_axis',(0.,0.,1.));
#19918=DIRECTION('ref_axis',(1.,0.,0.));
#19919=DIRECTION('center_axis',(0.,0.,1.));
#19920=DIRECTION('ref_axis',(0.374606593415912,-0.927183854566787,0.));
#19921=DIRECTION('center_axis',(0.,0.,1.));
#19922=DIRECTION('ref_axis',(1.,0.,0.));
#19923=DIRECTION('center_axis',(0.,0.,-1.));
#19924=DIRECTION('ref_axis',(-0.309016994374947,0.951056516295154,0.));
#19925=DIRECTION('center_axis',(0.,0.,1.));
#19926=DIRECTION('ref_axis',(1.,0.,0.));
#19927=DIRECTION('center_axis',(0.,0.,-1.));
#19928=DIRECTION('ref_axis',(-0.241921895599667,0.970295726275997,0.));
#19929=DIRECTION('center_axis',(0.,0.,1.));
#19930=DIRECTION('ref_axis',(1.,0.,0.));
#19931=DIRECTION('center_axis',(0.,0.,-1.));
#19932=DIRECTION('ref_axis',(-0.17364817766693,0.984807753012208,0.));
#19933=DIRECTION('center_axis',(0.,0.,1.));
#19934=DIRECTION('ref_axis',(1.,0.,0.));
#19935=DIRECTION('center_axis',(0.,0.,-1.));
#19936=DIRECTION('ref_axis',(-0.104528463267653,0.994521895368273,0.));
#19937=DIRECTION('center_axis',(0.,0.,1.));
#19938=DIRECTION('ref_axis',(1.,0.,0.));
#19939=DIRECTION('center_axis',(0.,0.,1.));
#19940=DIRECTION('ref_axis',(0.0348994967025013,-0.999390827019096,0.));
#19941=DIRECTION('center_axis',(0.,0.,1.));
#19942=DIRECTION('ref_axis',(1.,0.,0.));
#19943=DIRECTION('center_axis',(0.,0.,-1.));
#19944=DIRECTION('ref_axis',(0.0348994967025008,0.999390827019096,0.));
#19945=DIRECTION('center_axis',(0.,0.,1.));
#19946=DIRECTION('ref_axis',(-1.,0.,0.));
#19947=DIRECTION('center_axis',(0.,0.,-1.));
#19948=DIRECTION('ref_axis',(0.104528463267653,0.994521895368273,0.));
#19949=DIRECTION('center_axis',(0.,0.,1.));
#19950=DIRECTION('ref_axis',(-1.,0.,0.));
#19951=DIRECTION('center_axis',(0.,0.,-1.));
#19952=DIRECTION('ref_axis',(0.17364817766693,0.984807753012208,0.));
#19953=DIRECTION('center_axis',(0.,0.,1.));
#19954=DIRECTION('ref_axis',(-1.,0.,0.));
#19955=DIRECTION('center_axis',(0.,0.,-1.));
#19956=DIRECTION('ref_axis',(0.241921895599668,0.970295726275997,0.));
#19957=DIRECTION('center_axis',(0.,0.,1.));
#19958=DIRECTION('ref_axis',(-1.,0.,0.));
#19959=DIRECTION('center_axis',(0.,0.,1.));
#19960=DIRECTION('ref_axis',(-0.309016994374948,-0.951056516295154,0.));
#19961=DIRECTION('center_axis',(0.,0.,1.));
#19962=DIRECTION('ref_axis',(-1.,0.,0.));
#19963=DIRECTION('center_axis',(0.,0.,-1.));
#19964=DIRECTION('ref_axis',(0.374606593415912,0.927183854566787,0.));
#19965=DIRECTION('center_axis',(0.,0.,1.));
#19966=DIRECTION('ref_axis',(-1.,0.,0.));
#19967=DIRECTION('center_axis',(0.,0.,-1.));
#19968=DIRECTION('ref_axis',(0.438371146789078,0.898794046299167,0.));
#19969=DIRECTION('center_axis',(0.,0.,1.));
#19970=DIRECTION('ref_axis',(-1.,0.,0.));
#19971=DIRECTION('center_axis',(0.,0.,-1.));
#19972=DIRECTION('ref_axis',(0.5,0.866025403784438,0.));
#19973=DIRECTION('center_axis',(0.,0.,1.));
#19974=DIRECTION('ref_axis',(-1.,0.,0.));
#19975=DIRECTION('center_axis',(0.,0.,-1.));
#19976=DIRECTION('ref_axis',(0.559192903470747,0.829037572555042,0.));
#19977=DIRECTION('center_axis',(0.,0.,1.));
#19978=DIRECTION('ref_axis',(-1.,0.,0.));
#19979=DIRECTION('center_axis',(0.,0.,-1.));
#19980=DIRECTION('ref_axis',(0.615661475325658,0.788010753606722,0.));
#19981=DIRECTION('center_axis',(0.,0.,1.));
#19982=DIRECTION('ref_axis',(-1.,0.,0.));
#19983=DIRECTION('center_axis',(0.,0.,1.));
#19984=DIRECTION('ref_axis',(-0.669130606358858,-0.743144825477394,0.));
#19985=DIRECTION('center_axis',(0.,0.,1.));
#19986=DIRECTION('ref_axis',(-1.,0.,0.));
#19987=DIRECTION('center_axis',(0.,0.,-1.));
#19988=DIRECTION('ref_axis',(0.719339800338651,0.694658370458997,0.));
#19989=DIRECTION('center_axis',(0.,0.,1.));
#19990=DIRECTION('ref_axis',(-1.,0.,0.));
#19991=DIRECTION('center_axis',(0.,0.,-1.));
#19992=DIRECTION('ref_axis',(0.766044443118978,0.642787609686539,0.));
#19993=DIRECTION('center_axis',(0.,0.,1.));
#19994=DIRECTION('ref_axis',(-1.,0.,0.));
#19995=DIRECTION('center_axis',(0.,0.,-1.));
#19996=DIRECTION('ref_axis',(0.809016994374948,0.587785252292473,0.));
#19997=DIRECTION('center_axis',(0.,0.,1.));
#19998=DIRECTION('ref_axis',(-1.,0.,0.));
#19999=DIRECTION('center_axis',(0.,0.,-1.));
#20000=DIRECTION('ref_axis',(1.,0.,0.));
#20001=DIRECTION('center_axis',(0.,0.,1.));
#20002=DIRECTION('ref_axis',(0.96126169593832,0.275637355816994,0.));
#20003=DIRECTION('',(0.,0.,-1.));
#20004=DIRECTION('center_axis',(0.,0.,1.));
#20005=DIRECTION('ref_axis',(-0.961261695938319,-0.275637355816999,0.));
#20006=DIRECTION('',(0.,0.,1.));
#20007=DIRECTION('center_axis',(-0.971378440778616,0.237537207170802,0.));
#20008=DIRECTION('ref_axis',(0.,0.,1.));
#20009=DIRECTION('',(0.,0.,1.));
#20010=DIRECTION('',(-0.237537207170802,-0.971378440778616,0.));
#20011=DIRECTION('center_axis',(-0.969193219910856,-0.246301649362784,0.));
#20012=DIRECTION('ref_axis',(0.,0.,1.));
#20013=DIRECTION('',(0.,0.,1.));
#20014=DIRECTION('',(0.246301649362784,-0.969193219910856,0.));
#20015=DIRECTION('',(0.,0.,-1.));
#20016=DIRECTION('center_axis',(0.,0.,-1.));
#20017=DIRECTION('ref_axis',(0.719339800338651,0.694658370458997,0.));
#20018=DIRECTION('center_axis',(0.,0.,1.));
#20019=DIRECTION('ref_axis',(0.719339800338651,0.694658370458997,0.));
#20020=DIRECTION('center_axis',(0.,0.,1.));
#20021=DIRECTION('ref_axis',(0.719339800338677,0.69465837045897,0.));
#20022=DIRECTION('center_axis',(0.,0.,1.));
#20023=DIRECTION('ref_axis',(-0.719339800338651,-0.694658370458997,0.));
#20024=DIRECTION('',(0.,0.,1.));
#20025=DIRECTION('center_axis',(-0.279975964635093,-0.960007009988286,0.));
#20026=DIRECTION('ref_axis',(0.,0.,-1.));
#20027=DIRECTION('',(0.960007009988286,-0.279975964635093,0.));
#20028=DIRECTION('',(0.,0.,-1.));
#20029=DIRECTION('center_axis',(-0.984013448475508,-0.178094169526516,0.));
#20030=DIRECTION('ref_axis',(0.,0.,1.));
#20031=DIRECTION('',(0.,0.,1.));
#20032=DIRECTION('',(0.178094169526516,-0.984013448475508,0.));
#20033=DIRECTION('',(0.,0.,-1.));
#20034=DIRECTION('center_axis',(0.,0.,-1.));
#20035=DIRECTION('ref_axis',(0.766044443118978,0.642787609686539,0.));
#20036=DIRECTION('center_axis',(0.,0.,1.));
#20037=DIRECTION('ref_axis',(0.766044443118978,0.642787609686539,0.));
#20038=DIRECTION('center_axis',(0.,0.,1.));
#20039=DIRECTION('ref_axis',(0.766044443118982,0.642787609686535,0.));
#20040=DIRECTION('center_axis',(0.,0.,1.));
#20041=DIRECTION('ref_axis',(-0.766044443118978,-0.642787609686539,0.));
#20042=DIRECTION('',(0.,0.,1.));
#20043=DIRECTION('center_axis',(-0.346260661043498,-0.938138345135578,0.));
#20044=DIRECTION('ref_axis',(0.,0.,-1.));
#20045=DIRECTION('',(0.938138345135578,-0.346260661043498,0.));
#20046=DIRECTION('',(0.,0.,-1.));
#20047=DIRECTION('center_axis',(-0.994039662431923,-0.109019032798079,0.));
#20048=DIRECTION('ref_axis',(0.,0.,1.));
#20049=DIRECTION('',(0.,0.,1.));
#20050=DIRECTION('',(0.109019032798079,-0.994039662431923,0.));
#20051=DIRECTION('',(0.,0.,-1.));
#20052=DIRECTION('center_axis',(0.,0.,-1.));
#20053=DIRECTION('ref_axis',(0.809016994374947,0.587785252292473,0.));
#20054=DIRECTION('center_axis',(0.,0.,1.));
#20055=DIRECTION('ref_axis',(0.809016994374948,0.587785252292473,0.));
#20056=DIRECTION('center_axis',(0.,0.,1.));
#20057=DIRECTION('ref_axis',(0.809016994374978,0.587785252292431,0.));
#20058=DIRECTION('center_axis',(0.,0.,1.));
#20059=DIRECTION('ref_axis',(-0.809016994374948,-0.587785252292473,0.));
#20060=DIRECTION('',(0.,0.,1.));
#20061=DIRECTION('center_axis',(-0.999223015073487,-0.0394127663004103,
0.));
#20062=DIRECTION('ref_axis',(0.,0.,1.));
#20063=DIRECTION('',(0.,0.,1.));
#20064=DIRECTION('',(0.0394127663004103,-0.999223015073487,0.));
#20065=DIRECTION('center_axis',(0.,0.,1.));
#20066=DIRECTION('ref_axis',(1.,0.,0.));
#20067=DIRECTION('center_axis',(0.,0.,-1.));
#20068=DIRECTION('ref_axis',(-1.,0.,0.));
#20069=DIRECTION('',(0.,0.,-1.));
#20070=DIRECTION('center_axis',(0.,0.,1.));
#20071=DIRECTION('ref_axis',(1.,0.,0.));
#20072=DIRECTION('center_axis',(0.,0.,1.));
#20073=DIRECTION('ref_axis',(-1.,0.,0.));
#20074=DIRECTION('center_axis',(-0.410858410316832,-0.911699164566869,0.));
#20075=DIRECTION('ref_axis',(0.,0.,-1.));
#20076=DIRECTION('',(0.911699164566869,-0.410858410316832,0.));
#20077=DIRECTION('center_axis',(0.203491887231396,-0.979076632256641,0.));
#20078=DIRECTION('ref_axis',(0.,0.,-1.));
#20079=DIRECTION('',(0.979076632256641,0.203491887231396,0.));
#20080=DIRECTION('',(0.,0.,-1.));
#20081=DIRECTION('',(0.,0.,1.));
#20082=DIRECTION('center_axis',(0.,0.,1.));
#20083=DIRECTION('ref_axis',(-1.,0.,0.));
#20084=DIRECTION('center_axis',(0.,0.,-1.));
#20085=DIRECTION('ref_axis',(-1.,0.,0.));
#20086=DIRECTION('center_axis',(0.,0.,1.));
#20087=DIRECTION('ref_axis',(1.,0.,0.));
#20088=DIRECTION('center_axis',(0.,0.,1.));
#20089=DIRECTION('ref_axis',(1.,0.,0.));
#20090=DIRECTION('',(0.,0.,1.));
#20091=DIRECTION('center_axis',(-0.785222157581598,-0.61921414974377,0.));
#20092=DIRECTION('ref_axis',(0.,0.,1.));
#20093=DIRECTION('',(0.61921414974377,-0.785222157581598,0.));
#20094=DIRECTION('',(0.,0.,-1.));
#20095=DIRECTION('center_axis',(0.134699257830269,-0.990886527277455,0.));
#20096=DIRECTION('ref_axis',(0.,0.,-1.));
#20097=DIRECTION('',(0.990886527277455,0.134699257830269,0.));
#20098=DIRECTION('',(0.,0.,-1.));
#20099=DIRECTION('',(0.,0.,1.));
#20100=DIRECTION('center_axis',(0.,0.,1.));
#20101=DIRECTION('ref_axis',(-1.,0.,0.));
#20102=DIRECTION('center_axis',(0.,0.,-1.));
#20103=DIRECTION('ref_axis',(-1.,0.,0.));
#20104=DIRECTION('center_axis',(0.,0.,1.));
#20105=DIRECTION('ref_axis',(1.,0.,0.));
#20106=DIRECTION('center_axis',(0.,0.,1.));
#20107=DIRECTION('ref_axis',(1.,0.,0.));
#20108=DIRECTION('',(0.,0.,1.));
#20109=DIRECTION('center_axis',(-0.826503591449449,-0.562931446377943,0.));
#20110=DIRECTION('ref_axis',(0.,0.,1.));
#20111=DIRECTION('',(0.562931446377943,-0.826503591449449,0.));
#20112=DIRECTION('',(0.,0.,-1.));
#20113=DIRECTION('center_axis',(0.0652503871845092,-0.997868922740994,0.));
#20114=DIRECTION('ref_axis',(0.,0.,-1.));
#20115=DIRECTION('',(0.997868922740994,0.0652503871845092,0.));
#20116=DIRECTION('',(0.,0.,-1.));
#20117=DIRECTION('',(0.,0.,1.));
#20118=DIRECTION('center_axis',(0.,0.,1.));
#20119=DIRECTION('ref_axis',(-1.,0.,0.));
#20120=DIRECTION('center_axis',(0.,0.,-1.));
#20121=DIRECTION('ref_axis',(-1.,0.,0.));
#20122=DIRECTION('center_axis',(0.,0.,1.));
#20123=DIRECTION('ref_axis',(1.,0.,0.));
#20124=DIRECTION('center_axis',(0.,0.,1.));
#20125=DIRECTION('ref_axis',(1.,0.,0.));
#20126=DIRECTION('',(0.,0.,1.));
#20127=DIRECTION('center_axis',(-0.863758382899603,-0.503906197591043,0.));
#20128=DIRECTION('ref_axis',(0.,0.,1.));
#20129=DIRECTION('',(0.503906197591043,-0.863758382899603,0.));
#20130=DIRECTION('',(0.,0.,-1.));
#20131=DIRECTION('center_axis',(-0.0045163767884607,-0.999989801118344,
0.));
#20132=DIRECTION('ref_axis',(0.,0.,-1.));
#20133=DIRECTION('',(0.999989801118344,-0.0045163767884607,0.));
#20134=DIRECTION('',(0.,0.,-1.));
#20135=DIRECTION('',(0.,0.,1.));
#20136=DIRECTION('center_axis',(0.,0.,1.));
#20137=DIRECTION('ref_axis',(-1.,0.,0.));
#20138=DIRECTION('center_axis',(0.,0.,-1.));
#20139=DIRECTION('ref_axis',(-1.,0.,0.));
#20140=DIRECTION('center_axis',(0.,0.,1.));
#20141=DIRECTION('ref_axis',(1.,0.,0.));
#20142=DIRECTION('center_axis',(0.,0.,1.));
#20143=DIRECTION('ref_axis',(1.,0.,0.));
#20144=DIRECTION('',(0.,0.,1.));
#20145=DIRECTION('center_axis',(-0.896805030332968,-0.44242596846194,0.));
#20146=DIRECTION('ref_axis',(0.,0.,1.));
#20147=DIRECTION('',(0.44242596846194,-0.896805030332968,0.));
#20148=DIRECTION('',(0.,0.,-1.));
#20149=DIRECTION('center_axis',(-0.0742611374274884,-0.997238829703284,
0.));
#20150=DIRECTION('ref_axis',(0.,0.,-1.));
#20151=DIRECTION('',(0.997238829703284,-0.0742611374274884,0.));
#20152=DIRECTION('',(0.,0.,-1.));
#20153=DIRECTION('',(0.,0.,1.));
#20154=DIRECTION('center_axis',(0.,0.,1.));
#20155=DIRECTION('ref_axis',(-1.,0.,0.));
#20156=DIRECTION('center_axis',(0.,0.,-1.));
#20157=DIRECTION('ref_axis',(-1.,0.,0.));
#20158=DIRECTION('center_axis',(0.,0.,1.));
#20159=DIRECTION('ref_axis',(1.,0.,0.));
#20160=DIRECTION('center_axis',(0.,0.,1.));
#20161=DIRECTION('ref_axis',(1.,0.,0.));
#20162=DIRECTION('',(0.,0.,1.));
#20163=DIRECTION('center_axis',(-0.925482533805075,-0.378790284486995,0.));
#20164=DIRECTION('ref_axis',(0.,0.,1.));
#20165=DIRECTION('',(0.378790284486995,-0.925482533805075,0.));
#20166=DIRECTION('',(0.,0.,-1.));
#20167=DIRECTION('center_axis',(-0.143644105269881,-0.989629410952007,0.));
#20168=DIRECTION('ref_axis',(0.,0.,-1.));
#20169=DIRECTION('',(0.989629410952007,-0.143644105269881,0.));
#20170=DIRECTION('',(0.,0.,-1.));
#20171=DIRECTION('',(0.,0.,1.));
#20172=DIRECTION('center_axis',(0.,0.,1.));
#20173=DIRECTION('ref_axis',(-1.,0.,0.));
#20174=DIRECTION('center_axis',(0.,0.,-1.));
#20175=DIRECTION('ref_axis',(-1.,0.,0.));
#20176=DIRECTION('center_axis',(0.,0.,1.));
#20177=DIRECTION('ref_axis',(1.,0.,0.));
#20178=DIRECTION('center_axis',(0.,0.,1.));
#20179=DIRECTION('ref_axis',(1.,0.,0.));
#20180=DIRECTION('',(0.,0.,1.));
#20181=DIRECTION('center_axis',(-0.212327253470465,-0.977198617187769,0.));
#20182=DIRECTION('ref_axis',(0.,0.,-1.));
#20183=DIRECTION('',(0.,0.,1.));
#20184=DIRECTION('',(0.977198617187769,-0.212327253470465,0.));
#20185=DIRECTION('',(0.,0.,-1.));
#20186=DIRECTION('center_axis',(0.,0.,1.));
#20187=DIRECTION('ref_axis',(-1.,0.,0.));
#20188=DIRECTION('center_axis',(0.,0.,-1.));
#20189=DIRECTION('ref_axis',(-1.,0.,0.));
#20190=DIRECTION('center_axis',(0.,0.,1.));
#20191=DIRECTION('ref_axis',(-1.,0.,0.));
#20192=DIRECTION('center_axis',(0.,0.,-1.));
#20193=DIRECTION('ref_axis',(-1.,0.,0.));
#20194=DIRECTION('center_axis',(0.,0.,1.));
#20195=DIRECTION('ref_axis',(-1.,0.,0.));
#20196=DIRECTION('center_axis',(0.,0.,-1.));
#20197=DIRECTION('ref_axis',(-1.,0.,0.));
#20198=DIRECTION('center_axis',(0.,0.,1.));
#20199=DIRECTION('ref_axis',(1.,0.,0.));
#20200=DIRECTION('center_axis',(0.,0.,1.));
#20201=DIRECTION('ref_axis',(1.,0.,0.));
#20202=DIRECTION('center_axis',(0.,0.,1.));
#20203=DIRECTION('ref_axis',(1.,0.,0.));
#20204=DIRECTION('center_axis',(0.,0.,1.));
#20205=DIRECTION('ref_axis',(1.,0.,0.));
#20206=DIRECTION('center_axis',(0.,0.,1.));
#20207=DIRECTION('ref_axis',(1.,0.,0.));
#20208=DIRECTION('center_axis',(0.,0.,1.));
#20209=DIRECTION('ref_axis',(1.,0.,0.));
#20210=DIRECTION('center_axis',(-0.949651179401724,-0.313309172321709,0.));
#20211=DIRECTION('ref_axis',(0.,0.,1.));
#20212=DIRECTION('',(0.313309172321709,-0.949651179401724,0.));
#20213=DIRECTION('',(0.,0.,-1.));
#20214=DIRECTION('center_axis',(0.,0.,-1.));
#20215=DIRECTION('ref_axis',(0.374606593415912,0.927183854566787,0.));
#20216=DIRECTION('center_axis',(0.,0.,1.));
#20217=DIRECTION('ref_axis',(0.374606593415912,0.927183854566787,0.));
#20218=DIRECTION('center_axis',(0.,0.,-1.));
#20219=DIRECTION('ref_axis',(0.438371146789078,0.898794046299167,0.));
#20220=DIRECTION('center_axis',(0.,0.,1.));
#20221=DIRECTION('ref_axis',(0.438371146789078,0.898794046299167,0.));
#20222=DIRECTION('center_axis',(0.,0.,-1.));
#20223=DIRECTION('ref_axis',(0.5,0.866025403784438,0.));
#20224=DIRECTION('center_axis',(0.,0.,1.));
#20225=DIRECTION('ref_axis',(0.5,0.866025403784438,0.));
#20226=DIRECTION('center_axis',(0.,0.,-1.));
#20227=DIRECTION('ref_axis',(0.559192903470747,0.829037572555042,0.));
#20228=DIRECTION('center_axis',(0.,0.,1.));
#20229=DIRECTION('ref_axis',(0.559192903470747,0.829037572555042,0.));
#20230=DIRECTION('center_axis',(0.,0.,-1.));
#20231=DIRECTION('ref_axis',(0.615661475325658,0.788010753606722,0.));
#20232=DIRECTION('center_axis',(0.,0.,1.));
#20233=DIRECTION('ref_axis',(0.615661475325658,0.788010753606722,0.));
#20234=DIRECTION('center_axis',(0.,0.,1.));
#20235=DIRECTION('ref_axis',(0.66913060635886,0.743144825477393,0.));
#20236=DIRECTION('center_axis',(0.,0.,1.));
#20237=DIRECTION('ref_axis',(-0.669130606358858,-0.743144825477394,0.));
#20238=DIRECTION('center_axis',(0.,0.,1.));
#20239=DIRECTION('ref_axis',(0.615661475325709,0.788010753606683,0.));
#20240=DIRECTION('center_axis',(0.,0.,1.));
#20241=DIRECTION('ref_axis',(-0.615661475325658,-0.788010753606722,0.));
#20242=DIRECTION('center_axis',(0.,0.,1.));
#20243=DIRECTION('ref_axis',(0.559192903470803,0.829037572555004,0.));
#20244=DIRECTION('center_axis',(0.,0.,1.));
#20245=DIRECTION('ref_axis',(-0.559192903470747,-0.829037572555042,0.));
#20246=DIRECTION('center_axis',(0.,0.,1.));
#20247=DIRECTION('ref_axis',(0.5,0.866025403784439,0.));
#20248=DIRECTION('center_axis',(0.,0.,1.));
#20249=DIRECTION('ref_axis',(-0.5,-0.866025403784438,0.));
#20250=DIRECTION('center_axis',(0.,0.,1.));
#20251=DIRECTION('ref_axis',(0.438371146789079,0.898794046299166,0.));
#20252=DIRECTION('center_axis',(0.,0.,1.));
#20253=DIRECTION('ref_axis',(-0.438371146789078,-0.898794046299167,0.));
#20254=DIRECTION('center_axis',(0.,0.,1.));
#20255=DIRECTION('ref_axis',(0.374606593415967,0.927183854566765,0.));
#20256=DIRECTION('center_axis',(0.,0.,1.));
#20257=DIRECTION('ref_axis',(-0.374606593415912,-0.927183854566787,0.));
#20258=DIRECTION('center_axis',(-0.526083754912358,-0.850432762078998,0.));
#20259=DIRECTION('ref_axis',(0.,0.,1.));
#20260=DIRECTION('',(0.,0.,1.));
#20261=DIRECTION('',(0.850432762078998,-0.526083754912358,0.));
#20262=DIRECTION('',(0.,0.,-1.));
#20263=DIRECTION('center_axis',(0.,0.,-1.));
#20264=DIRECTION('ref_axis',(0.0348994967025008,0.999390827019096,0.));
#20265=DIRECTION('center_axis',(0.,0.,1.));
#20266=DIRECTION('ref_axis',(0.0348994967025008,0.999390827019096,0.));
#20267=DIRECTION('center_axis',(0.,0.,1.));
#20268=DIRECTION('ref_axis',(0.0348994967025657,0.999390827019093,0.));
#20269=DIRECTION('center_axis',(0.,0.,1.));
#20270=DIRECTION('ref_axis',(-0.0348994967025008,-0.999390827019096,0.));
#20271=DIRECTION('',(0.,0.,1.));
#20272=DIRECTION('center_axis',(0.465479050687347,-0.885058898249832,0.));
#20273=DIRECTION('ref_axis',(0.,0.,-1.));
#20274=DIRECTION('',(0.885058898249832,0.465479050687346,0.));
#20275=DIRECTION('',(0.,0.,-1.));
#20276=DIRECTION('center_axis',(0.,0.,1.));
#20277=DIRECTION('ref_axis',(-1.,0.,0.));
#20278=DIRECTION('center_axis',(0.,0.,-1.));
#20279=DIRECTION('ref_axis',(-1.,0.,0.));
#20280=DIRECTION('center_axis',(-0.584125431965383,-0.811663402976415,0.));
#20281=DIRECTION('ref_axis',(0.,0.,1.));
#20282=DIRECTION('',(0.,0.,1.));
#20283=DIRECTION('',(0.811663402976415,-0.584125431965383,0.));
#20284=DIRECTION('',(0.,0.,-1.));
#20285=DIRECTION('center_axis',(0.,0.,-1.));
#20286=DIRECTION('ref_axis',(0.104528463267653,0.994521895368273,0.));
#20287=DIRECTION('center_axis',(0.,0.,1.));
#20288=DIRECTION('ref_axis',(0.104528463267653,0.994521895368273,0.));
#20289=DIRECTION('center_axis',(0.,0.,1.));
#20290=DIRECTION('ref_axis',(0.104528463267748,0.994521895368263,0.));
#20291=DIRECTION('center_axis',(0.,0.,1.));
#20292=DIRECTION('ref_axis',(-0.104528463267653,-0.994521895368273,0.));
#20293=DIRECTION('',(0.,0.,1.));
#20294=DIRECTION('center_axis',(0.402606579317095,-0.91537311643427,0.));
#20295=DIRECTION('ref_axis',(0.,0.,-1.));
#20296=DIRECTION('',(0.91537311643427,0.402606579317095,0.));
#20297=DIRECTION('',(0.,0.,-1.));
#20298=DIRECTION('center_axis',(-0.639321308629955,-0.76893970136265,0.));
#20299=DIRECTION('ref_axis',(0.,0.,1.));
#20300=DIRECTION('',(0.,0.,1.));
#20301=DIRECTION('',(0.76893970136265,-0.639321308629955,0.));
#20302=DIRECTION('',(0.,0.,-1.));
#20303=DIRECTION('center_axis',(0.,0.,-1.));
#20304=DIRECTION('ref_axis',(0.17364817766693,0.984807753012208,0.));
#20305=DIRECTION('center_axis',(0.,0.,1.));
#20306=DIRECTION('ref_axis',(0.17364817766693,0.984807753012208,0.));
#20307=DIRECTION('center_axis',(0.,0.,1.));
#20308=DIRECTION('ref_axis',(0.173648177666931,0.984807753012208,0.));
#20309=DIRECTION('center_axis',(0.,0.,1.));
#20310=DIRECTION('ref_axis',(-0.17364817766693,-0.984807753012208,0.));
#20311=DIRECTION('',(0.,0.,1.));
#20312=DIRECTION('center_axis',(0.337772649161909,-0.941227728808574,0.));
#20313=DIRECTION('ref_axis',(0.,0.,-1.));
#20314=DIRECTION('',(0.941227728808574,0.337772649161909,0.));
#20315=DIRECTION('',(0.,0.,-1.));
#20316=DIRECTION('center_axis',(-0.691402476143223,-0.722469802817405,0.));
#20317=DIRECTION('ref_axis',(0.,0.,1.));
#20318=DIRECTION('',(0.,0.,1.));
#20319=DIRECTION('',(0.722469802817405,-0.691402476143223,0.));
#20320=DIRECTION('',(0.,0.,-1.));
#20321=DIRECTION('center_axis',(0.,0.,-1.));
#20322=DIRECTION('ref_axis',(0.241921895599668,0.970295726275996,0.));
#20323=DIRECTION('center_axis',(0.,0.,1.));
#20324=DIRECTION('ref_axis',(0.241921895599668,0.970295726275996,0.));
#20325=DIRECTION('center_axis',(0.,0.,1.));
#20326=DIRECTION('ref_axis',(0.241921895599671,0.970295726275996,0.));
#20327=DIRECTION('center_axis',(0.,0.,1.));
#20328=DIRECTION('ref_axis',(-0.241921895599668,-0.970295726275996,0.));
#20329=DIRECTION('',(0.,0.,1.));
#20330=DIRECTION('center_axis',(-0.740115200292399,-0.672480104015087,0.));
#20331=DIRECTION('ref_axis',(0.,0.,1.));
#20332=DIRECTION('',(0.,0.,1.));
#20333=DIRECTION('',(0.672480104015087,-0.740115200292399,0.));
#20334=DIRECTION('',(0.,0.,-1.));
#20335=DIRECTION('center_axis',(0.,0.,1.));
#20336=DIRECTION('ref_axis',(1.,0.,0.));
#20337=DIRECTION('center_axis',(0.,0.,-1.));
#20338=DIRECTION('ref_axis',(-1.,0.,0.));
#20339=DIRECTION('',(0.,0.,-1.));
#20340=DIRECTION('center_axis',(0.,0.,1.));
#20341=DIRECTION('ref_axis',(1.,0.,0.));
#20342=DIRECTION('center_axis',(0.,0.,1.));
#20343=DIRECTION('ref_axis',(-1.,0.,0.));
#20344=DIRECTION('center_axis',(0.271293124613069,-0.962496774299882,0.));
#20345=DIRECTION('ref_axis',(0.,0.,-1.));
#20346=DIRECTION('',(0.962496774299882,0.271293124613069,0.));
#20347=DIRECTION('center_axis',(0.785222157581596,-0.619214149743772,0.));
#20348=DIRECTION('ref_axis',(0.,0.,-1.));
#20349=DIRECTION('',(0.619214149743772,0.785222157581596,0.));
#20350=DIRECTION('',(0.,0.,-1.));
#20351=DIRECTION('',(0.,0.,1.));
#20352=DIRECTION('center_axis',(0.,0.,1.));
#20353=DIRECTION('ref_axis',(1.,0.,0.));
#20354=DIRECTION('center_axis',(0.,0.,-1.));
#20355=DIRECTION('ref_axis',(1.,0.,0.));
#20356=DIRECTION('center_axis',(0.,0.,1.));
#20357=DIRECTION('ref_axis',(1.,0.,0.));
#20358=DIRECTION('center_axis',(0.,0.,1.));
#20359=DIRECTION('ref_axis',(1.,0.,0.));
#20360=DIRECTION('',(0.,0.,1.));
#20361=DIRECTION('center_axis',(-0.203491887231601,-0.979076632256598,0.));
#20362=DIRECTION('ref_axis',(0.,0.,-1.));
#20363=DIRECTION('',(0.979076632256598,-0.203491887231601,0.));
#20364=DIRECTION('',(0.,0.,-1.));
#20365=DIRECTION('center_axis',(0.740115200292476,-0.672480104015002,0.));
#20366=DIRECTION('ref_axis',(0.,0.,-1.));
#20367=DIRECTION('',(0.672480104015002,0.740115200292476,0.));
#20368=DIRECTION('',(0.,0.,-1.));
#20369=DIRECTION('',(0.,0.,1.));
#20370=DIRECTION('center_axis',(0.,0.,1.));
#20371=DIRECTION('ref_axis',(1.,0.,0.));
#20372=DIRECTION('center_axis',(0.,0.,-1.));
#20373=DIRECTION('ref_axis',(1.,0.,0.));
#20374=DIRECTION('center_axis',(0.,0.,1.));
#20375=DIRECTION('ref_axis',(1.,0.,0.));
#20376=DIRECTION('center_axis',(0.,0.,1.));
#20377=DIRECTION('ref_axis',(1.,0.,0.));
#20378=DIRECTION('',(0.,0.,1.));
#20379=DIRECTION('center_axis',(-0.27129312461336,-0.9624967742998,0.));
#20380=DIRECTION('ref_axis',(0.,0.,-1.));
#20381=DIRECTION('',(0.9624967742998,-0.27129312461336,0.));
#20382=DIRECTION('',(0.,0.,-1.));
#20383=DIRECTION('center_axis',(0.691402476143227,-0.722469802817401,0.));
#20384=DIRECTION('ref_axis',(0.,0.,-1.));
#20385=DIRECTION('',(0.722469802817401,0.691402476143227,0.));
#20386=DIRECTION('',(0.,0.,-1.));
#20387=DIRECTION('',(0.,0.,1.));
#20388=DIRECTION('center_axis',(0.,0.,1.));
#20389=DIRECTION('ref_axis',(1.,0.,0.));
#20390=DIRECTION('center_axis',(0.,0.,-1.));
#20391=DIRECTION('ref_axis',(1.,0.,0.));
#20392=DIRECTION('center_axis',(0.,0.,1.));
#20393=DIRECTION('ref_axis',(1.,0.,0.));
#20394=DIRECTION('center_axis',(0.,0.,1.));
#20395=DIRECTION('ref_axis',(1.,0.,0.));
#20396=DIRECTION('',(0.,0.,1.));
#20397=DIRECTION('center_axis',(-0.337772649162104,-0.941227728808504,0.));
#20398=DIRECTION('ref_axis',(0.,0.,-1.));
#20399=DIRECTION('',(0.941227728808504,-0.337772649162104,0.));
#20400=DIRECTION('',(0.,0.,-1.));
#20401=DIRECTION('center_axis',(0.639321308629947,-0.768939701362657,0.));
#20402=DIRECTION('ref_axis',(0.,0.,-1.));
#20403=DIRECTION('',(0.768939701362657,0.639321308629947,0.));
#20404=DIRECTION('',(0.,0.,-1.));
#20405=DIRECTION('',(0.,0.,1.));
#20406=DIRECTION('center_axis',(0.,0.,1.));
#20407=DIRECTION('ref_axis',(1.,0.,0.));
#20408=DIRECTION('center_axis',(0.,0.,-1.));
#20409=DIRECTION('ref_axis',(1.,0.,0.));
#20410=DIRECTION('center_axis',(0.,0.,1.));
#20411=DIRECTION('ref_axis',(1.,0.,0.));
#20412=DIRECTION('center_axis',(0.,0.,1.));
#20413=DIRECTION('ref_axis',(1.,0.,0.));
#20414=DIRECTION('',(0.,0.,1.));
#20415=DIRECTION('center_axis',(-0.402606579317095,-0.91537311643427,0.));
#20416=DIRECTION('ref_axis',(0.,0.,-1.));
#20417=DIRECTION('',(0.91537311643427,-0.402606579317095,0.));
#20418=DIRECTION('',(0.,0.,-1.));
#20419=DIRECTION('center_axis',(0.584125431965637,-0.811663402976233,0.));
#20420=DIRECTION('ref_axis',(0.,0.,-1.));
#20421=DIRECTION('',(0.811663402976233,0.584125431965637,0.));
#20422=DIRECTION('',(0.,0.,-1.));
#20423=DIRECTION('',(0.,0.,1.));
#20424=DIRECTION('center_axis',(0.,0.,1.));
#20425=DIRECTION('ref_axis',(1.,0.,0.));
#20426=DIRECTION('center_axis',(0.,0.,-1.));
#20427=DIRECTION('ref_axis',(1.,0.,0.));
#20428=DIRECTION('center_axis',(0.,0.,1.));
#20429=DIRECTION('ref_axis',(1.,0.,0.));
#20430=DIRECTION('center_axis',(0.,0.,1.));
#20431=DIRECTION('ref_axis',(1.,0.,0.));
#20432=DIRECTION('',(0.,0.,1.));
#20433=DIRECTION('center_axis',(0.526083754912359,-0.850432762078998,0.));
#20434=DIRECTION('ref_axis',(0.,0.,-1.));
#20435=DIRECTION('',(0.,0.,1.));
#20436=DIRECTION('',(0.850432762078998,0.526083754912359,0.));
#20437=DIRECTION('',(0.,0.,-1.));
#20438=DIRECTION('center_axis',(0.,0.,1.));
#20439=DIRECTION('ref_axis',(1.,0.,0.));
#20440=DIRECTION('center_axis',(0.,0.,-1.));
#20441=DIRECTION('ref_axis',(1.,0.,0.));
#20442=DIRECTION('center_axis',(0.,0.,1.));
#20443=DIRECTION('ref_axis',(-1.,0.,0.));
#20444=DIRECTION('center_axis',(0.,0.,-1.));
#20445=DIRECTION('ref_axis',(-1.,0.,0.));
#20446=DIRECTION('center_axis',(0.,0.,1.));
#20447=DIRECTION('ref_axis',(-1.,0.,0.));
#20448=DIRECTION('center_axis',(0.,0.,-1.));
#20449=DIRECTION('ref_axis',(-1.,0.,0.));
#20450=DIRECTION('center_axis',(0.,0.,1.));
#20451=DIRECTION('ref_axis',(1.,0.,0.));
#20452=DIRECTION('center_axis',(0.,0.,1.));
#20453=DIRECTION('ref_axis',(1.,0.,0.));
#20454=DIRECTION('center_axis',(0.,0.,1.));
#20455=DIRECTION('ref_axis',(1.,0.,0.));
#20456=DIRECTION('center_axis',(0.,0.,1.));
#20457=DIRECTION('ref_axis',(1.,0.,0.));
#20458=DIRECTION('center_axis',(0.,0.,1.));
#20459=DIRECTION('ref_axis',(1.,0.,0.));
#20460=DIRECTION('center_axis',(0.,0.,1.));
#20461=DIRECTION('ref_axis',(1.,0.,0.));
#20462=DIRECTION('center_axis',(0.,0.,1.));
#20463=DIRECTION('ref_axis',(1.,0.,0.));
#20464=DIRECTION('center_axis',(0.,0.,1.));
#20465=DIRECTION('ref_axis',(1.,0.,0.));
#20466=DIRECTION('center_axis',(-0.465479050687165,-0.885058898249928,0.));
#20467=DIRECTION('ref_axis',(0.,0.,-1.));
#20468=DIRECTION('',(0.885058898249927,-0.465479050687165,0.));
#20469=DIRECTION('',(0.,0.,-1.));
#20470=DIRECTION('center_axis',(0.,0.,-1.));
#20471=DIRECTION('ref_axis',(-0.309016994374947,0.951056516295154,0.));
#20472=DIRECTION('center_axis',(0.,0.,1.));
#20473=DIRECTION('ref_axis',(-0.309016994374947,0.951056516295154,0.));
#20474=DIRECTION('center_axis',(0.,0.,-1.));
#20475=DIRECTION('ref_axis',(-0.241921895599667,0.970295726275997,0.));
#20476=DIRECTION('center_axis',(0.,0.,1.));
#20477=DIRECTION('ref_axis',(-0.241921895599667,0.970295726275997,0.));
#20478=DIRECTION('center_axis',(0.,0.,-1.));
#20479=DIRECTION('ref_axis',(-0.17364817766693,0.984807753012208,0.));
#20480=DIRECTION('center_axis',(0.,0.,1.));
#20481=DIRECTION('ref_axis',(-0.17364817766693,0.984807753012208,0.));
#20482=DIRECTION('center_axis',(0.,0.,-1.));
#20483=DIRECTION('ref_axis',(-0.104528463267653,0.994521895368273,0.));
#20484=DIRECTION('center_axis',(0.,0.,1.));
#20485=DIRECTION('ref_axis',(-0.104528463267653,0.994521895368273,0.));
#20486=DIRECTION('center_axis',(0.,0.,1.));
#20487=DIRECTION('ref_axis',(-0.0348994967025032,0.999390827019096,0.));
#20488=DIRECTION('center_axis',(0.,0.,1.));
#20489=DIRECTION('ref_axis',(0.0348994967025013,-0.999390827019096,0.));
#20490=DIRECTION('center_axis',(0.,0.,1.));
#20491=DIRECTION('ref_axis',(-0.104528463267655,0.994521895368273,0.));
#20492=DIRECTION('center_axis',(0.,0.,1.));
#20493=DIRECTION('ref_axis',(0.104528463267653,-0.994521895368273,0.));
#20494=DIRECTION('center_axis',(0.,0.,1.));
#20495=DIRECTION('ref_axis',(-0.173648177666993,0.984807753012197,0.));
#20496=DIRECTION('center_axis',(0.,0.,1.));
#20497=DIRECTION('ref_axis',(0.17364817766693,-0.984807753012208,0.));
#20498=DIRECTION('center_axis',(0.,0.,1.));
#20499=DIRECTION('ref_axis',(-0.241921895599764,0.970295726275972,0.));
#20500=DIRECTION('center_axis',(0.,0.,1.));
#20501=DIRECTION('ref_axis',(0.241921895599667,-0.970295726275997,0.));
#20502=DIRECTION('center_axis',(0.,0.,1.));
#20503=DIRECTION('ref_axis',(-0.309016994374908,0.951056516295166,0.));
#20504=DIRECTION('center_axis',(0.,0.,1.));
#20505=DIRECTION('ref_axis',(0.309016994374947,-0.951056516295154,0.));
#20506=DIRECTION('center_axis',(0.212327253470672,-0.977198617187725,0.));
#20507=DIRECTION('ref_axis',(0.,0.,-1.));
#20508=DIRECTION('',(0.,0.,1.));
#20509=DIRECTION('',(0.977198617187725,0.212327253470672,0.));
#20510=DIRECTION('',(0.,0.,-1.));
#20511=DIRECTION('center_axis',(0.,0.,-1.));
#20512=DIRECTION('ref_axis',(-0.669130606358858,0.743144825477395,0.));
#20513=DIRECTION('center_axis',(0.,0.,1.));
#20514=DIRECTION('ref_axis',(-0.669130606358858,0.743144825477395,0.));
#20515=DIRECTION('center_axis',(0.,0.,1.));
#20516=DIRECTION('ref_axis',(-0.669130606358858,0.743144825477394,0.));
#20517=DIRECTION('center_axis',(0.,0.,1.));
#20518=DIRECTION('ref_axis',(0.669130606358858,-0.743144825477395,0.));
#20519=DIRECTION('',(0.,0.,1.));
#20520=DIRECTION('center_axis',(0.949651179401661,-0.313309172321899,0.));
#20521=DIRECTION('ref_axis',(0.,0.,-1.));
#20522=DIRECTION('',(0.313309172321899,0.949651179401661,0.));
#20523=DIRECTION('',(0.,0.,-1.));
#20524=DIRECTION('center_axis',(0.143644105269891,-0.989629410952005,0.));
#20525=DIRECTION('ref_axis',(0.,0.,-1.));
#20526=DIRECTION('',(0.,0.,1.));
#20527=DIRECTION('',(0.989629410952005,0.143644105269891,0.));
#20528=DIRECTION('',(0.,0.,-1.));
#20529=DIRECTION('center_axis',(0.,0.,-1.));
#20530=DIRECTION('ref_axis',(-0.615661475325659,0.788010753606722,0.));
#20531=DIRECTION('center_axis',(0.,0.,1.));
#20532=DIRECTION('ref_axis',(-0.615661475325659,0.788010753606722,0.));
#20533=DIRECTION('center_axis',(0.,0.,1.));
#20534=DIRECTION('ref_axis',(-0.615661475325708,0.788010753606683,0.));
#20535=DIRECTION('center_axis',(0.,0.,1.));
#20536=DIRECTION('ref_axis',(0.615661475325659,-0.788010753606722,0.));
#20537=DIRECTION('',(0.,0.,1.));
#20538=DIRECTION('center_axis',(0.925482533805075,-0.378790284486995,0.));
#20539=DIRECTION('ref_axis',(0.,0.,-1.));
#20540=DIRECTION('',(0.378790284486995,0.925482533805075,0.));
#20541=DIRECTION('',(0.,0.,-1.));
#20542=DIRECTION('center_axis',(0.0742611374277114,-0.997238829703268,0.));
#20543=DIRECTION('ref_axis',(0.,0.,-1.));
#20544=DIRECTION('',(0.,0.,1.));
#20545=DIRECTION('',(0.997238829703268,0.0742611374277114,0.));
#20546=DIRECTION('',(0.,0.,-1.));
#20547=DIRECTION('center_axis',(0.,0.,-1.));
#20548=DIRECTION('ref_axis',(-0.559192903470747,0.829037572555042,0.));
#20549=DIRECTION('center_axis',(0.,0.,1.));
#20550=DIRECTION('ref_axis',(-0.559192903470747,0.829037572555042,0.));
#20551=DIRECTION('center_axis',(0.,0.,1.));
#20552=DIRECTION('ref_axis',(-0.559192903470747,0.829037572555042,0.));
#20553=DIRECTION('center_axis',(0.,0.,1.));
#20554=DIRECTION('ref_axis',(0.559192903470747,-0.829037572555042,0.));
#20555=DIRECTION('',(0.,0.,1.));
#20556=DIRECTION('center_axis',(0.896805030332968,-0.44242596846194,0.));
#20557=DIRECTION('ref_axis',(0.,0.,-1.));
#20558=DIRECTION('',(0.442425968461939,0.896805030332968,0.));
#20559=DIRECTION('',(0.,0.,-1.));
#20560=DIRECTION('center_axis',(0.0045163767882446,-0.999989801118345,0.));
#20561=DIRECTION('ref_axis',(0.,0.,-1.));
#20562=DIRECTION('',(0.,0.,1.));
#20563=DIRECTION('',(0.999989801118345,0.0045163767882446,0.));
#20564=DIRECTION('',(0.,0.,-1.));
#20565=DIRECTION('center_axis',(0.,0.,-1.));
#20566=DIRECTION('ref_axis',(-0.5,0.866025403784438,0.));
#20567=DIRECTION('center_axis',(0.,0.,1.));
#20568=DIRECTION('ref_axis',(-0.5,0.866025403784439,0.));
#20569=DIRECTION('center_axis',(0.,0.,1.));
#20570=DIRECTION('ref_axis',(-0.500000000000006,0.866025403784435,0.));
#20571=DIRECTION('center_axis',(0.,0.,1.));
#20572=DIRECTION('ref_axis',(0.5,-0.866025403784439,0.));
#20573=DIRECTION('',(0.,0.,1.));
#20574=DIRECTION('center_axis',(0.863758382899708,-0.503906197590862,0.));
#20575=DIRECTION('ref_axis',(0.,0.,-1.));
#20576=DIRECTION('',(0.503906197590862,0.863758382899708,0.));
#20577=DIRECTION('',(0.,0.,-1.));
#20578=DIRECTION('center_axis',(-0.0652503871847299,-0.997868922740979,
0.));
#20579=DIRECTION('ref_axis',(0.,0.,-1.));
#20580=DIRECTION('',(0.,0.,1.));
#20581=DIRECTION('',(0.997868922740979,-0.0652503871847299,0.));
#20582=DIRECTION('',(0.,0.,-1.));
#20583=DIRECTION('center_axis',(0.,0.,-1.));
#20584=DIRECTION('ref_axis',(-0.438371146789077,0.898794046299167,0.));
#20585=DIRECTION('center_axis',(0.,0.,1.));
#20586=DIRECTION('ref_axis',(-0.438371146789077,0.898794046299167,0.));
#20587=DIRECTION('center_axis',(0.,0.,1.));
#20588=DIRECTION('ref_axis',(-0.438371146789136,0.898794046299139,0.));
#20589=DIRECTION('center_axis',(0.,0.,1.));
#20590=DIRECTION('ref_axis',(0.438371146789077,-0.898794046299167,0.));
#20591=DIRECTION('',(0.,0.,1.));
#20592=DIRECTION('center_axis',(-0.134699257830059,-0.990886527277484,0.));
#20593=DIRECTION('ref_axis',(0.,0.,-1.));
#20594=DIRECTION('',(0.,0.,1.));
#20595=DIRECTION('',(0.990886527277484,-0.134699257830059,0.));
#20596=DIRECTION('',(0.,0.,-1.));
#20597=DIRECTION('center_axis',(0.,0.,1.));
#20598=DIRECTION('ref_axis',(1.,0.,0.));
#20599=DIRECTION('center_axis',(0.,0.,-1.));
#20600=DIRECTION('ref_axis',(1.,0.,0.));
#20601=DIRECTION('',(0.,0.,-1.));
#20602=DIRECTION('center_axis',(0.,0.,1.));
#20603=DIRECTION('ref_axis',(1.,0.,0.));
#20604=DIRECTION('center_axis',(0.,0.,1.));
#20605=DIRECTION('ref_axis',(1.,0.,0.));
#20606=DIRECTION('center_axis',(0.826503591449449,-0.562931446377943,0.));
#20607=DIRECTION('ref_axis',(0.,0.,-1.));
#20608=DIRECTION('',(0.562931446377943,0.826503591449449,0.));
#20609=DIRECTION('center_axis',(0.999538253627158,0.0303855152329264,0.));
#20610=DIRECTION('ref_axis',(0.,0.,-1.));
#20611=DIRECTION('',(-0.0303855152329264,0.999538253627158,0.));
#20612=DIRECTION('',(0.,0.,-1.));
#20613=DIRECTION('',(0.,0.,1.));
#20614=DIRECTION('center_axis',(0.,0.,1.));
#20615=DIRECTION('ref_axis',(1.,0.,0.));
#20616=DIRECTION('center_axis',(0.,0.,-1.));
#20617=DIRECTION('ref_axis',(1.,0.,0.));
#20618=DIRECTION('center_axis',(0.,0.,1.));
#20619=DIRECTION('ref_axis',(1.,0.,0.));
#20620=DIRECTION('center_axis',(0.,0.,1.));
#20621=DIRECTION('ref_axis',(1.,0.,0.));
#20622=DIRECTION('',(0.,0.,1.));
#20623=DIRECTION('center_axis',(0.473454498714615,-0.880818277312008,0.));
#20624=DIRECTION('ref_axis',(0.,0.,-1.));
#20625=DIRECTION('',(0.880818277312008,0.473454498714615,0.));
#20626=DIRECTION('',(0.,0.,-1.));
#20627=DIRECTION('center_axis',(0.999223015073487,-0.0394127663004103,0.));
#20628=DIRECTION('ref_axis',(0.,0.,-1.));
#20629=DIRECTION('',(0.0394127663004103,0.999223015073487,0.));
#20630=DIRECTION('',(0.,0.,-1.));
#20631=DIRECTION('',(0.,0.,1.));
#20632=DIRECTION('center_axis',(0.,0.,1.));
#20633=DIRECTION('ref_axis',(1.,0.,0.));
#20634=DIRECTION('center_axis',(0.,0.,-1.));
#20635=DIRECTION('ref_axis',(1.,0.,0.));
#20636=DIRECTION('center_axis',(0.,0.,1.));
#20637=DIRECTION('ref_axis',(1.,0.,0.));
#20638=DIRECTION('center_axis',(0.,0.,1.));
#20639=DIRECTION('ref_axis',(1.,0.,0.));
#20640=DIRECTION('',(0.,0.,1.));
#20641=DIRECTION('center_axis',(0.410858410317009,-0.911699164566789,0.));
#20642=DIRECTION('ref_axis',(0.,0.,-1.));
#20643=DIRECTION('',(0.911699164566789,0.410858410317009,0.));
#20644=DIRECTION('',(0.,0.,-1.));
#20645=DIRECTION('center_axis',(0.994039662431923,-0.10901903279808,0.));
#20646=DIRECTION('ref_axis',(0.,0.,-1.));
#20647=DIRECTION('',(0.10901903279808,0.994039662431923,0.));
#20648=DIRECTION('',(0.,0.,-1.));
#20649=DIRECTION('',(0.,0.,1.));
#20650=DIRECTION('center_axis',(0.,0.,1.));
#20651=DIRECTION('ref_axis',(1.,0.,0.));
#20652=DIRECTION('center_axis',(0.,0.,-1.));
#20653=DIRECTION('ref_axis',(1.,0.,0.));
#20654=DIRECTION('center_axis',(0.,0.,1.));
#20655=DIRECTION('ref_axis',(1.,0.,0.));
#20656=DIRECTION('center_axis',(0.,0.,1.));
#20657=DIRECTION('ref_axis',(1.,0.,0.));
#20658=DIRECTION('',(0.,0.,1.));
#20659=DIRECTION('center_axis',(0.346260661043305,-0.938138345135649,0.));
#20660=DIRECTION('ref_axis',(0.,0.,-1.));
#20661=DIRECTION('',(0.938138345135649,0.346260661043305,0.));
#20662=DIRECTION('',(0.,0.,-1.));
#20663=DIRECTION('center_axis',(0.984013448475546,-0.178094169526304,0.));
#20664=DIRECTION('ref_axis',(0.,0.,-1.));
#20665=DIRECTION('',(0.178094169526304,0.984013448475546,0.));
#20666=DIRECTION('',(0.,0.,-1.));
#20667=DIRECTION('',(0.,0.,1.));
#20668=DIRECTION('center_axis',(0.,0.,1.));
#20669=DIRECTION('ref_axis',(1.,0.,0.));
#20670=DIRECTION('center_axis',(0.,0.,-1.));
#20671=DIRECTION('ref_axis',(1.,0.,0.));
#20672=DIRECTION('center_axis',(0.,0.,1.));
#20673=DIRECTION('ref_axis',(1.,0.,0.));
#20674=DIRECTION('center_axis',(0.,0.,1.));
#20675=DIRECTION('ref_axis',(1.,0.,0.));
#20676=DIRECTION('',(0.,0.,1.));
#20677=DIRECTION('center_axis',(0.969193219910809,-0.246301649362969,0.));
#20678=DIRECTION('ref_axis',(0.,0.,-1.));
#20679=DIRECTION('',(0.,0.,1.));
#20680=DIRECTION('',(0.246301649362969,0.969193219910809,0.));
#20681=DIRECTION('',(0.,0.,-1.));
#20682=DIRECTION('center_axis',(0.,0.,1.));
#20683=DIRECTION('ref_axis',(1.,0.,0.));
#20684=DIRECTION('center_axis',(0.,0.,-1.));
#20685=DIRECTION('ref_axis',(1.,0.,0.));
#20686=DIRECTION('center_axis',(0.,0.,1.));
#20687=DIRECTION('ref_axis',(1.,0.,0.));
#20688=DIRECTION('center_axis',(0.,0.,-1.));
#20689=DIRECTION('ref_axis',(1.,0.,0.));
#20690=DIRECTION('center_axis',(0.,0.,1.));
#20691=DIRECTION('ref_axis',(1.,0.,0.));
#20692=DIRECTION('center_axis',(0.,0.,-1.));
#20693=DIRECTION('ref_axis',(1.,0.,0.));
#20694=DIRECTION('center_axis',(0.,0.,1.));
#20695=DIRECTION('ref_axis',(1.,0.,0.));
#20696=DIRECTION('center_axis',(0.,0.,-1.));
#20697=DIRECTION('ref_axis',(1.,0.,0.));
#20698=DIRECTION('center_axis',(0.,0.,1.));
#20699=DIRECTION('ref_axis',(1.,0.,0.));
#20700=DIRECTION('center_axis',(0.,0.,-1.));
#20701=DIRECTION('ref_axis',(1.,0.,0.));
#20702=DIRECTION('center_axis',(0.,0.,1.));
#20703=DIRECTION('ref_axis',(1.,0.,0.));
#20704=DIRECTION('center_axis',(0.,0.,1.));
#20705=DIRECTION('ref_axis',(1.,0.,0.));
#20706=DIRECTION('center_axis',(0.,0.,1.));
#20707=DIRECTION('ref_axis',(1.,0.,0.));
#20708=DIRECTION('center_axis',(0.,0.,1.));
#20709=DIRECTION('ref_axis',(1.,0.,0.));
#20710=DIRECTION('center_axis',(0.,0.,1.));
#20711=DIRECTION('ref_axis',(1.,0.,0.));
#20712=DIRECTION('center_axis',(0.,0.,1.));
#20713=DIRECTION('ref_axis',(1.,0.,0.));
#20714=DIRECTION('center_axis',(0.,0.,1.));
#20715=DIRECTION('ref_axis',(1.,0.,0.));
#20716=DIRECTION('center_axis',(0.,0.,1.));
#20717=DIRECTION('ref_axis',(1.,0.,0.));
#20718=DIRECTION('center_axis',(0.,0.,1.));
#20719=DIRECTION('ref_axis',(1.,0.,0.));
#20720=DIRECTION('center_axis',(0.,0.,1.));
#20721=DIRECTION('ref_axis',(1.,0.,0.));
#20722=DIRECTION('center_axis',(0.279975964635192,-0.960007009988257,0.));
#20723=DIRECTION('ref_axis',(0.,0.,-1.));
#20724=DIRECTION('',(0.960007009988257,0.279975964635192,0.));
#20725=DIRECTION('',(0.,0.,-1.));
#20726=DIRECTION('center_axis',(0.,0.,-1.));
#20727=DIRECTION('ref_axis',(-0.848048096156426,0.529919264233205,0.));
#20728=DIRECTION('center_axis',(0.,0.,1.));
#20729=DIRECTION('ref_axis',(-0.848048096156426,0.529919264233205,0.));
#20730=DIRECTION('center_axis',(0.,0.,-1.));
#20731=DIRECTION('ref_axis',(-0.809016994374947,0.587785252292473,0.));
#20732=DIRECTION('center_axis',(0.,0.,1.));
#20733=DIRECTION('ref_axis',(-0.809016994374947,0.587785252292473,0.));
#20734=DIRECTION('center_axis',(0.,0.,-1.));
#20735=DIRECTION('ref_axis',(-0.766044443118978,0.64278760968654,0.));
#20736=DIRECTION('center_axis',(0.,0.,1.));
#20737=DIRECTION('ref_axis',(-0.766044443118978,0.64278760968654,0.));
#20738=DIRECTION('center_axis',(0.,0.,1.));
#20739=DIRECTION('ref_axis',(-0.719339800338695,0.694658370458952,0.));
#20740=DIRECTION('center_axis',(0.,0.,1.));
#20741=DIRECTION('ref_axis',(0.719339800338651,-0.694658370458998,0.));
#20742=DIRECTION('center_axis',(0.,0.,1.));
#20743=DIRECTION('ref_axis',(-0.766044443118978,0.64278760968654,0.));
#20744=DIRECTION('center_axis',(0.,0.,1.));
#20745=DIRECTION('ref_axis',(0.766044443118978,-0.64278760968654,0.));
#20746=DIRECTION('center_axis',(0.,0.,1.));
#20747=DIRECTION('ref_axis',(-0.809016994374946,0.587785252292475,0.));
#20748=DIRECTION('center_axis',(0.,0.,1.));
#20749=DIRECTION('ref_axis',(0.809016994374947,-0.587785252292473,0.));
#20750=DIRECTION('center_axis',(0.,0.,1.));
#20751=DIRECTION('ref_axis',(-0.848048096156458,0.529919264233154,0.));
#20752=DIRECTION('center_axis',(0.,0.,1.));
#20753=DIRECTION('ref_axis',(0.848048096156426,-0.529919264233205,0.));
#20754=DIRECTION('center_axis',(0.831554643148335,-0.555442954279236,0.));
#20755=DIRECTION('ref_axis',(0.,0.,-1.));
#20756=DIRECTION('',(0.,0.,1.));
#20757=DIRECTION('',(0.555442954279236,0.831554643148335,0.));
#20758=DIRECTION('',(0.,0.,-1.));
#20759=DIRECTION('center_axis',(0.,0.,-1.));
#20760=DIRECTION('ref_axis',(-0.997564050259824,0.0697564737441256,0.));
#20761=DIRECTION('center_axis',(0.,0.,1.));
#20762=DIRECTION('ref_axis',(-0.997564050259824,0.0697564737441256,0.));
#20763=DIRECTION('center_axis',(0.,0.,1.));
#20764=DIRECTION('ref_axis',(-0.997564050259824,0.0697564737441253,0.));
#20765=DIRECTION('center_axis',(0.,0.,1.));
#20766=DIRECTION('ref_axis',(0.997564050259824,-0.0697564737441256,0.));
#20767=DIRECTION('',(0.,0.,1.));
#20768=DIRECTION('center_axis',(0.900764728877051,0.434307383325513,0.));
#20769=DIRECTION('ref_axis',(0.,0.,-1.));
#20770=DIRECTION('',(-0.434307383325513,0.900764728877051,0.));
#20771=DIRECTION('',(0.,0.,-1.));
#20772=DIRECTION('center_axis',(0.,0.,1.));
#20773=DIRECTION('ref_axis',(1.,0.,0.));
#20774=DIRECTION('center_axis',(0.,0.,-1.));
#20775=DIRECTION('ref_axis',(1.,0.,0.));
#20776=DIRECTION('center_axis',(0.790783275975002,-0.612096242790497,0.));
#20777=DIRECTION('ref_axis',(0.,0.,-1.));
#20778=DIRECTION('',(0.,0.,1.));
#20779=DIRECTION('',(0.612096242790497,0.790783275975002,0.));
#20780=DIRECTION('',(0.,0.,-1.));
#20781=DIRECTION('center_axis',(0.,0.,-1.));
#20782=DIRECTION('ref_axis',(-0.99026806874157,0.139173100960066,0.));
#20783=DIRECTION('center_axis',(0.,0.,1.));
#20784=DIRECTION('ref_axis',(-0.99026806874157,0.139173100960066,0.));
#20785=DIRECTION('center_axis',(0.,0.,1.));
#20786=DIRECTION('ref_axis',(-0.990268068741562,0.139173100960128,0.));
#20787=DIRECTION('center_axis',(0.,0.,1.));
#20788=DIRECTION('ref_axis',(0.99026806874157,-0.139173100960066,0.));
#20789=DIRECTION('',(0.,0.,1.));
#20790=DIRECTION('center_axis',(0.928866262851607,0.370415261208404,0.));
#20791=DIRECTION('ref_axis',(0.,0.,-1.));
#20792=DIRECTION('',(-0.370415261208404,0.928866262851607,0.));
#20793=DIRECTION('',(0.,0.,-1.));
#20794=DIRECTION('center_axis',(0.746159292170273,-0.665767459934741,0.));
#20795=DIRECTION('ref_axis',(0.,0.,-1.));
#20796=DIRECTION('',(0.,0.,1.));
#20797=DIRECTION('',(0.665767459934741,0.746159292170273,0.));
#20798=DIRECTION('',(0.,0.,-1.));
#20799=DIRECTION('center_axis',(0.,0.,-1.));
#20800=DIRECTION('ref_axis',(-0.978147600733806,0.20791169081776,0.));
#20801=DIRECTION('center_axis',(0.,0.,1.));
#20802=DIRECTION('ref_axis',(-0.978147600733806,0.20791169081776,0.));
#20803=DIRECTION('center_axis',(0.,0.,1.));
#20804=DIRECTION('ref_axis',(-0.978147600733805,0.207911690817762,0.));
#20805=DIRECTION('center_axis',(0.,0.,1.));
#20806=DIRECTION('ref_axis',(0.978147600733806,-0.20791169081776,0.));
#20807=DIRECTION('',(0.,0.,1.));
#20808=DIRECTION('center_axis',(0.952442453762932,0.304718513172479,0.));
#20809=DIRECTION('ref_axis',(0.,0.,-1.));
#20810=DIRECTION('',(-0.304718513172479,0.952442453762931,0.));
#20811=DIRECTION('',(0.,0.,-1.));
#20812=DIRECTION('center_axis',(0.697900095297528,-0.716195124937124,0.));
#20813=DIRECTION('ref_axis',(0.,0.,-1.));
#20814=DIRECTION('',(0.,0.,1.));
#20815=DIRECTION('',(0.716195124937124,0.697900095297528,0.));
#20816=DIRECTION('',(0.,0.,-1.));
#20817=DIRECTION('center_axis',(0.,0.,-1.));
#20818=DIRECTION('ref_axis',(-0.961261695938319,0.275637355816999,0.));
#20819=DIRECTION('center_axis',(0.,0.,1.));
#20820=DIRECTION('ref_axis',(-0.961261695938319,0.275637355816999,0.));
#20821=DIRECTION('center_axis',(0.,0.,1.));
#20822=DIRECTION('ref_axis',(-0.961261695938347,0.2756373558169,0.));
#20823=DIRECTION('center_axis',(0.,0.,1.));
#20824=DIRECTION('ref_axis',(0.961261695938319,-0.275637355816999,0.));
#20825=DIRECTION('',(0.,0.,1.));
#20826=DIRECTION('center_axis',(0.971378440778617,0.237537207170797,0.));
#20827=DIRECTION('ref_axis',(0.,0.,-1.));
#20828=DIRECTION('',(-0.237537207170797,0.971378440778617,0.));
#20829=DIRECTION('',(0.,0.,-1.));
#20830=DIRECTION('center_axis',(0.646240799313603,-0.763133559282066,0.));
#20831=DIRECTION('ref_axis',(0.,0.,-1.));
#20832=DIRECTION('',(0.,0.,1.));
#20833=DIRECTION('',(0.763133559282066,0.646240799313603,0.));
#20834=DIRECTION('',(0.,0.,-1.));
#20835=DIRECTION('center_axis',(0.,0.,-1.));
#20836=DIRECTION('ref_axis',(-0.939692620785908,0.342020143325669,0.));
#20837=DIRECTION('center_axis',(0.,0.,1.));
#20838=DIRECTION('ref_axis',(-0.939692620785908,0.342020143325669,0.));
#20839=DIRECTION('center_axis',(0.,0.,1.));
#20840=DIRECTION('ref_axis',(-0.939692620785885,0.342020143325732,0.));
#20841=DIRECTION('center_axis',(0.,0.,1.));
#20842=DIRECTION('ref_axis',(0.939692620785908,-0.342020143325669,0.));
#20843=DIRECTION('',(0.,0.,1.));
#20844=DIRECTION('center_axis',(0.985581969673418,0.169198643773125,0.));
#20845=DIRECTION('ref_axis',(0.,0.,-1.));
#20846=DIRECTION('',(-0.169198643773125,0.985581969673418,0.));
#20847=DIRECTION('',(0.,0.,-1.));
#20848=DIRECTION('center_axis',(0.591433083115112,-0.80635408363631,0.));
#20849=DIRECTION('ref_axis',(0.,0.,-1.));
#20850=DIRECTION('',(0.,0.,1.));
#20851=DIRECTION('',(0.80635408363631,0.591433083115112,0.));
#20852=DIRECTION('',(0.,0.,-1.));
#20853=DIRECTION('center_axis',(0.,0.,-1.));
#20854=DIRECTION('ref_axis',(-0.913545457642601,0.4067366430758,0.));
#20855=DIRECTION('center_axis',(0.,0.,1.));
#20856=DIRECTION('ref_axis',(-0.913545457642601,0.4067366430758,0.));
#20857=DIRECTION('center_axis',(0.,0.,1.));
#20858=DIRECTION('ref_axis',(-0.913545457642558,0.406736643075896,0.));
#20859=DIRECTION('center_axis',(0.,0.,1.));
#20860=DIRECTION('ref_axis',(0.913545457642601,-0.4067366430758,0.));
#20861=DIRECTION('',(0.,0.,1.));
#20862=DIRECTION('center_axis',(0.533743964386317,-0.845646131949516,0.));
#20863=DIRECTION('ref_axis',(0.,0.,-1.));
#20864=DIRECTION('',(0.,0.,1.));
#20865=DIRECTION('',(0.845646131949516,0.533743964386317,0.));
#20866=DIRECTION('',(0.,0.,-1.));
#20867=DIRECTION('center_axis',(0.,0.,1.));
#20868=DIRECTION('ref_axis',(1.,0.,0.));
#20869=DIRECTION('center_axis',(0.,0.,-1.));
#20870=DIRECTION('ref_axis',(1.,0.,0.));
#20871=DIRECTION('',(0.,0.,-1.));
#20872=DIRECTION('center_axis',(0.,0.,1.));
#20873=DIRECTION('ref_axis',(1.,0.,0.));
#20874=DIRECTION('center_axis',(0.,0.,1.));
#20875=DIRECTION('ref_axis',(1.,0.,0.));
#20876=DIRECTION('center_axis',(0.994983842282363,0.100035761590676,0.));
#20877=DIRECTION('ref_axis',(0.,0.,-1.));
#20878=DIRECTION('',(-0.100035761590676,0.994983842282363,0.));
#20879=DIRECTION('center_axis',(0.746159292170123,0.66576745993491,0.));
#20880=DIRECTION('ref_axis',(0.,0.,-1.));
#20881=DIRECTION('',(-0.66576745993491,0.746159292170123,0.));
#20882=DIRECTION('',(0.,0.,-1.));
#20883=DIRECTION('',(0.,0.,1.));
#20884=DIRECTION('center_axis',(0.,0.,1.));
#20885=DIRECTION('ref_axis',(1.,0.,0.));
#20886=DIRECTION('center_axis',(0.,0.,-1.));
#20887=DIRECTION('ref_axis',(1.,0.,0.));
#20888=DIRECTION('center_axis',(0.,0.,1.));
#20889=DIRECTION('ref_axis',(1.,0.,0.));
#20890=DIRECTION('center_axis',(0.,0.,1.));
#20891=DIRECTION('ref_axis',(1.,0.,0.));
#20892=DIRECTION('',(0.,0.,1.));
#20893=DIRECTION('center_axis',(0.92886626285169,-0.370415261208196,0.));
#20894=DIRECTION('ref_axis',(0.,0.,-1.));
#20895=DIRECTION('',(0.370415261208196,0.928866262851689,0.));
#20896=DIRECTION('',(0.,0.,-1.));
#20897=DIRECTION('center_axis',(0.790783275974884,0.61209624279065,0.));
#20898=DIRECTION('ref_axis',(0.,0.,-1.));
#20899=DIRECTION('',(-0.61209624279065,0.790783275974884,0.));
#20900=DIRECTION('',(0.,0.,-1.));
#20901=DIRECTION('',(0.,0.,1.));
#20902=DIRECTION('center_axis',(0.,0.,1.));
#20903=DIRECTION('ref_axis',(1.,0.,0.));
#20904=DIRECTION('center_axis',(0.,0.,-1.));
#20905=DIRECTION('ref_axis',(1.,0.,0.));
#20906=DIRECTION('center_axis',(0.,0.,1.));
#20907=DIRECTION('ref_axis',(1.,0.,0.));
#20908=DIRECTION('center_axis',(0.,0.,1.));
#20909=DIRECTION('ref_axis',(1.,0.,0.));
#20910=DIRECTION('',(0.,0.,1.));
#20911=DIRECTION('center_axis',(0.900764728877053,-0.434307383325507,0.));
#20912=DIRECTION('ref_axis',(0.,0.,-1.));
#20913=DIRECTION('',(0.434307383325507,0.900764728877053,0.));
#20914=DIRECTION('',(0.,0.,-1.));
#20915=DIRECTION('center_axis',(0.831554643148452,0.555442954279061,0.));
#20916=DIRECTION('ref_axis',(0.,0.,-1.));
#20917=DIRECTION('',(-0.555442954279061,0.831554643148452,0.));
#20918=DIRECTION('',(0.,0.,-1.));
#20919=DIRECTION('',(0.,0.,1.));
#20920=DIRECTION('center_axis',(0.,0.,1.));
#20921=DIRECTION('ref_axis',(1.,0.,0.));
#20922=DIRECTION('center_axis',(0.,0.,-1.));
#20923=DIRECTION('ref_axis',(1.,0.,0.));
#20924=DIRECTION('center_axis',(0.,0.,1.));
#20925=DIRECTION('ref_axis',(1.,0.,0.));
#20926=DIRECTION('center_axis',(0.,0.,1.));
#20927=DIRECTION('ref_axis',(1.,0.,0.));
#20928=DIRECTION('',(0.,0.,1.));
#20929=DIRECTION('center_axis',(0.868274759687958,0.496083603527489,0.));
#20930=DIRECTION('ref_axis',(0.,0.,-1.));
#20931=DIRECTION('',(0.,0.,1.));
#20932=DIRECTION('',(-0.496083603527489,0.868274759687958,0.));
#20933=DIRECTION('',(0.,0.,-1.));
#20934=DIRECTION('center_axis',(0.,0.,1.));
#20935=DIRECTION('ref_axis',(1.,0.,0.));
#20936=DIRECTION('center_axis',(0.,0.,-1.));
#20937=DIRECTION('ref_axis',(1.,0.,0.));
#20938=DIRECTION('center_axis',(0.,0.,1.));
#20939=DIRECTION('ref_axis',(1.,0.,0.));
#20940=DIRECTION('center_axis',(0.,0.,-1.));
#20941=DIRECTION('ref_axis',(1.,0.,0.));
#20942=DIRECTION('center_axis',(0.,0.,1.));
#20943=DIRECTION('ref_axis',(1.,0.,0.));
#20944=DIRECTION('center_axis',(0.,0.,-1.));
#20945=DIRECTION('ref_axis',(1.,0.,0.));
#20946=DIRECTION('center_axis',(0.,0.,1.));
#20947=DIRECTION('ref_axis',(1.,0.,0.));
#20948=DIRECTION('center_axis',(0.,0.,-1.));
#20949=DIRECTION('ref_axis',(1.,0.,0.));
#20950=DIRECTION('center_axis',(0.,0.,1.));
#20951=DIRECTION('ref_axis',(1.,0.,0.));
#20952=DIRECTION('center_axis',(0.,0.,-1.));
#20953=DIRECTION('ref_axis',(1.,0.,0.));
#20954=DIRECTION('center_axis',(0.,0.,1.));
#20955=DIRECTION('ref_axis',(1.,0.,0.));
#20956=DIRECTION('center_axis',(0.,0.,1.));
#20957=DIRECTION('ref_axis',(1.,0.,0.));
#20958=DIRECTION('center_axis',(0.,0.,1.));
#20959=DIRECTION('ref_axis',(1.,0.,0.));
#20960=DIRECTION('center_axis',(0.,0.,1.));
#20961=DIRECTION('ref_axis',(1.,0.,0.));
#20962=DIRECTION('center_axis',(0.,0.,1.));
#20963=DIRECTION('ref_axis',(1.,0.,0.));
#20964=DIRECTION('center_axis',(0.,0.,1.));
#20965=DIRECTION('ref_axis',(1.,0.,0.));
#20966=DIRECTION('center_axis',(0.,0.,1.));
#20967=DIRECTION('ref_axis',(1.,0.,0.));
#20968=DIRECTION('center_axis',(0.,0.,1.));
#20969=DIRECTION('ref_axis',(1.,0.,0.));
#20970=DIRECTION('center_axis',(0.,0.,1.));
#20971=DIRECTION('ref_axis',(1.,0.,0.));
#20972=DIRECTION('center_axis',(0.,0.,1.));
#20973=DIRECTION('ref_axis',(1.,0.,0.));
#20974=DIRECTION('center_axis',(0.,0.,1.));
#20975=DIRECTION('ref_axis',(1.,0.,0.));
#20976=DIRECTION('center_axis',(0.,0.,1.));
#20977=DIRECTION('ref_axis',(1.,0.,0.));
#20978=DIRECTION('center_axis',(0.868274759687958,-0.496083603527489,0.));
#20979=DIRECTION('ref_axis',(0.,0.,-1.));
#20980=DIRECTION('',(0.496083603527489,0.868274759687958,0.));
#20981=DIRECTION('',(0.,0.,-1.));
#20982=DIRECTION('center_axis',(0.,0.,-1.));
#20983=DIRECTION('ref_axis',(-0.99026806874157,-0.139173100960065,0.));
#20984=DIRECTION('center_axis',(0.,0.,1.));
#20985=DIRECTION('ref_axis',(-0.99026806874157,-0.139173100960065,0.));
#20986=DIRECTION('center_axis',(0.,0.,-1.));
#20987=DIRECTION('ref_axis',(-0.997564050259824,-0.0697564737441253,0.));
#20988=DIRECTION('center_axis',(0.,0.,1.));
#20989=DIRECTION('ref_axis',(-0.997564050259824,-0.0697564737441253,0.));
#20990=DIRECTION('center_axis',(0.,0.,1.));
#20991=DIRECTION('ref_axis',(-1.,-1.22464679914735E-16,0.));
#20992=DIRECTION('center_axis',(0.,0.,1.));
#20993=DIRECTION('ref_axis',(1.,0.,0.));
#20994=DIRECTION('center_axis',(0.,0.,1.));
#20995=DIRECTION('ref_axis',(-0.99756405025982,-0.0697564737441876,0.));
#20996=DIRECTION('center_axis',(0.,0.,1.));
#20997=DIRECTION('ref_axis',(0.997564050259824,0.0697564737441253,0.));
#20998=DIRECTION('center_axis',(0.,0.,1.));
#20999=DIRECTION('ref_axis',(-0.99026806874158,-0.139173100959998,0.));
#21000=DIRECTION('center_axis',(0.,0.,1.));
#21001=DIRECTION('ref_axis',(0.99026806874157,0.139173100960065,0.));
#21002=DIRECTION('center_axis',(0.984013448475508,0.178094169526516,0.));
#21003=DIRECTION('ref_axis',(0.,0.,-1.));
#21004=DIRECTION('',(0.,0.,1.));
#21005=DIRECTION('',(-0.178094169526516,0.984013448475508,0.));
#21006=DIRECTION('',(0.,0.,-1.));
#21007=DIRECTION('center_axis',(0.,0.,-1.));
#21008=DIRECTION('ref_axis',(-0.766044443118978,-0.642787609686539,0.));
#21009=DIRECTION('center_axis',(0.,0.,1.));
#21010=DIRECTION('ref_axis',(-0.766044443118978,-0.642787609686539,0.));
#21011=DIRECTION('center_axis',(0.,0.,1.));
#21012=DIRECTION('ref_axis',(-0.766044443118982,-0.642787609686535,0.));
#21013=DIRECTION('center_axis',(0.,0.,1.));
#21014=DIRECTION('ref_axis',(0.766044443118978,0.642787609686539,0.));
#21015=DIRECTION('',(0.,0.,1.));
#21016=DIRECTION('center_axis',(0.346260661043498,0.938138345135578,0.));
#21017=DIRECTION('ref_axis',(0.,0.,1.));
#21018=DIRECTION('',(-0.938138345135578,0.346260661043498,0.));
#21019=DIRECTION('',(0.,0.,-1.));
#21020=DIRECTION('center_axis',(0.994039662431945,0.109019032797875,0.));
#21021=DIRECTION('ref_axis',(0.,0.,-1.));
#21022=DIRECTION('',(0.,0.,1.));
#21023=DIRECTION('',(-0.109019032797875,0.994039662431945,0.));
#21024=DIRECTION('',(0.,0.,-1.));
#21025=DIRECTION('center_axis',(0.,0.,-1.));
#21026=DIRECTION('ref_axis',(-0.809016994374948,-0.587785252292473,0.));
#21027=DIRECTION('center_axis',(0.,0.,1.));
#21028=DIRECTION('ref_axis',(-0.809016994374948,-0.587785252292473,0.));
#21029=DIRECTION('center_axis',(0.,0.,1.));
#21030=DIRECTION('ref_axis',(-0.809016994374945,-0.587785252292477,0.));
#21031=DIRECTION('center_axis',(0.,0.,1.));
#21032=DIRECTION('ref_axis',(0.809016994374948,0.587785252292473,0.));
#21033=DIRECTION('',(0.,0.,1.));
#21034=DIRECTION('center_axis',(0.41085841031682,0.911699164566874,0.));
#21035=DIRECTION('ref_axis',(0.,0.,1.));
#21036=DIRECTION('',(-0.911699164566874,0.41085841031682,0.));
#21037=DIRECTION('',(0.,0.,-1.));
#21038=DIRECTION('center_axis',(0.999223015073487,0.0394127663004103,0.));
#21039=DIRECTION('ref_axis',(0.,0.,-1.));
#21040=DIRECTION('',(0.,0.,1.));
#21041=DIRECTION('',(-0.0394127663004103,0.999223015073487,0.));
#21042=DIRECTION('',(0.,0.,-1.));
#21043=DIRECTION('center_axis',(0.,0.,-1.));
#21044=DIRECTION('ref_axis',(-0.848048096156426,-0.529919264233205,0.));
#21045=DIRECTION('center_axis',(0.,0.,1.));
#21046=DIRECTION('ref_axis',(-0.848048096156426,-0.529919264233205,0.));
#21047=DIRECTION('center_axis',(0.,0.,1.));
#21048=DIRECTION('ref_axis',(-0.848048096156423,-0.529919264233209,0.));
#21049=DIRECTION('center_axis',(0.,0.,1.));
#21050=DIRECTION('ref_axis',(0.848048096156426,0.529919264233205,0.));
#21051=DIRECTION('',(0.,0.,1.));
#21052=DIRECTION('center_axis',(0.473454498714793,0.880818277311912,0.));
#21053=DIRECTION('ref_axis',(0.,0.,1.));
#21054=DIRECTION('',(-0.880818277311912,0.473454498714793,0.));
#21055=DIRECTION('',(0.,0.,-1.));
#21056=DIRECTION('center_axis',(0.999538253627158,-0.0303855152329264,0.));
#21057=DIRECTION('ref_axis',(0.,0.,-1.));
#21058=DIRECTION('',(0.,0.,1.));
#21059=DIRECTION('',(0.0303855152329264,0.999538253627158,0.));
#21060=DIRECTION('',(0.,0.,-1.));
#21061=DIRECTION('center_axis',(0.,0.,-1.));
#21062=DIRECTION('ref_axis',(-0.882947592858927,-0.469471562785891,0.));
#21063=DIRECTION('center_axis',(0.,0.,1.));
#21064=DIRECTION('ref_axis',(-0.882947592858927,-0.469471562785891,0.));
#21065=DIRECTION('center_axis',(0.,0.,1.));
#21066=DIRECTION('ref_axis',(-0.882947592858927,-0.469471562785891,0.));
#21067=DIRECTION('center_axis',(0.,0.,1.));
#21068=DIRECTION('ref_axis',(0.882947592858927,0.469471562785891,0.));
#21069=DIRECTION('',(0.,0.,1.));
#21070=DIRECTION('center_axis',(0.533743964386317,0.845646131949516,0.));
#21071=DIRECTION('ref_axis',(0.,0.,-1.));
#21072=DIRECTION('',(-0.845646131949516,0.533743964386317,0.));
#21073=DIRECTION('',(0.,0.,-1.));
#21074=DIRECTION('center_axis',(0.994983842282394,-0.100035761590367,0.));
#21075=DIRECTION('ref_axis',(0.,0.,-1.));
#21076=DIRECTION('',(0.,0.,1.));
#21077=DIRECTION('',(0.100035761590367,0.994983842282394,0.));
#21078=DIRECTION('',(0.,0.,-1.));
#21079=DIRECTION('center_axis',(0.,0.,-1.));
#21080=DIRECTION('ref_axis',(-0.913545457642601,-0.4067366430758,0.));
#21081=DIRECTION('center_axis',(0.,0.,1.));
#21082=DIRECTION('ref_axis',(-0.913545457642601,-0.4067366430758,0.));
#21083=DIRECTION('center_axis',(0.,0.,1.));
#21084=DIRECTION('ref_axis',(-0.913545457642598,-0.406736643075806,0.));
#21085=DIRECTION('center_axis',(0.,0.,1.));
#21086=DIRECTION('ref_axis',(0.913545457642601,0.4067366430758,0.));
#21087=DIRECTION('',(0.,0.,1.));
#21088=DIRECTION('center_axis',(0.591433083115112,0.80635408363631,0.));
#21089=DIRECTION('ref_axis',(0.,0.,-1.));
#21090=DIRECTION('',(-0.80635408363631,0.591433083115112,0.));
#21091=DIRECTION('',(0.,0.,-1.));
#21092=DIRECTION('center_axis',(0.985581969673453,-0.169198643772926,0.));
#21093=DIRECTION('ref_axis',(0.,0.,-1.));
#21094=DIRECTION('',(0.,0.,1.));
#21095=DIRECTION('',(0.169198643772926,0.985581969673453,0.));
#21096=DIRECTION('',(0.,0.,-1.));
#21097=DIRECTION('center_axis',(0.,0.,-1.));
#21098=DIRECTION('ref_axis',(-0.939692620785908,-0.342020143325669,0.));
#21099=DIRECTION('center_axis',(0.,0.,1.));
#21100=DIRECTION('ref_axis',(-0.939692620785908,-0.342020143325669,0.));
#21101=DIRECTION('center_axis',(0.,0.,1.));
#21102=DIRECTION('ref_axis',(-0.939692620785908,-0.342020143325671,0.));
#21103=DIRECTION('center_axis',(0.,0.,1.));
#21104=DIRECTION('ref_axis',(0.939692620785908,0.342020143325669,0.));
#21105=DIRECTION('',(0.,0.,1.));
#21106=DIRECTION('center_axis',(0.646240799313611,0.76313355928206,0.));
#21107=DIRECTION('ref_axis',(0.,0.,-1.));
#21108=DIRECTION('',(-0.76313355928206,0.646240799313611,0.));
#21109=DIRECTION('',(0.,0.,-1.));
#21110=DIRECTION('center_axis',(0.971378440778567,-0.237537207171004,0.));
#21111=DIRECTION('ref_axis',(0.,0.,-1.));
#21112=DIRECTION('',(0.,0.,1.));
#21113=DIRECTION('',(0.237537207171004,0.971378440778567,0.));
#21114=DIRECTION('',(0.,0.,-1.));
#21115=DIRECTION('center_axis',(0.,0.,-1.));
#21116=DIRECTION('ref_axis',(-0.961261695938319,-0.275637355816999,0.));
#21117=DIRECTION('center_axis',(0.,0.,1.));
#21118=DIRECTION('ref_axis',(-0.961261695938319,-0.275637355816999,0.));
#21119=DIRECTION('center_axis',(0.,0.,1.));
#21120=DIRECTION('ref_axis',(-0.96126169593832,-0.275637355816994,0.));
#21121=DIRECTION('center_axis',(0.,0.,1.));
#21122=DIRECTION('ref_axis',(0.961261695938319,0.275637355816999,0.));
#21123=DIRECTION('',(0.,0.,1.));
#21124=DIRECTION('center_axis',(0.952442453762929,-0.304718513172487,0.));
#21125=DIRECTION('ref_axis',(0.,0.,-1.));
#21126=DIRECTION('',(0.,0.,1.));
#21127=DIRECTION('',(0.304718513172487,0.952442453762929,0.));
#21128=DIRECTION('',(0.,0.,-1.));
#21129=DIRECTION('center_axis',(0.,0.,1.));
#21130=DIRECTION('ref_axis',(1.,0.,0.));
#21131=DIRECTION('center_axis',(0.,0.,-1.));
#21132=DIRECTION('ref_axis',(1.,0.,0.));
#21133=DIRECTION('',(0.,0.,-1.));
#21134=DIRECTION('center_axis',(0.,0.,1.));
#21135=DIRECTION('ref_axis',(1.,0.,0.));
#21136=DIRECTION('center_axis',(0.,0.,1.));
#21137=DIRECTION('ref_axis',(1.,0.,0.));
#21138=DIRECTION('center_axis',(0.697900095297593,0.71619512493706,0.));
#21139=DIRECTION('ref_axis',(0.,0.,-1.));
#21140=DIRECTION('',(-0.71619512493706,0.697900095297593,0.));
#21141=DIRECTION('center_axis',(0.143644105269892,0.989629410952005,0.));
#21142=DIRECTION('ref_axis',(0.,0.,1.));
#21143=DIRECTION('',(-0.989629410952005,0.143644105269892,0.));
#21144=DIRECTION('',(0.,0.,-1.));
#21145=DIRECTION('',(0.,0.,1.));
#21146=DIRECTION('center_axis',(0.,0.,1.));
#21147=DIRECTION('ref_axis',(1.,0.,0.));
#21148=DIRECTION('center_axis',(0.,0.,-1.));
#21149=DIRECTION('ref_axis',(1.,0.,0.));
#21150=DIRECTION('center_axis',(0.,0.,1.));
#21151=DIRECTION('ref_axis',(1.,0.,0.));
#21152=DIRECTION('center_axis',(0.,0.,1.));
#21153=DIRECTION('ref_axis',(1.,0.,0.));
#21154=DIRECTION('',(0.,0.,1.));
#21155=DIRECTION('center_axis',(0.949651179401728,0.313309172321697,0.));
#21156=DIRECTION('ref_axis',(0.,0.,-1.));
#21157=DIRECTION('',(-0.313309172321697,0.949651179401728,0.));
#21158=DIRECTION('',(0.,0.,-1.));
#21159=DIRECTION('center_axis',(0.212327253470465,0.977198617187769,0.));
#21160=DIRECTION('ref_axis',(0.,0.,1.));
#21161=DIRECTION('',(-0.977198617187769,0.212327253470465,0.));
#21162=DIRECTION('',(0.,0.,-1.));
#21163=DIRECTION('',(0.,0.,1.));
#21164=DIRECTION('center_axis',(0.,0.,1.));
#21165=DIRECTION('ref_axis',(1.,0.,0.));
#21166=DIRECTION('center_axis',(0.,0.,-1.));
#21167=DIRECTION('ref_axis',(1.,0.,0.));
#21168=DIRECTION('center_axis',(0.,0.,1.));
#21169=DIRECTION('ref_axis',(1.,0.,0.));
#21170=DIRECTION('center_axis',(0.,0.,1.));
#21171=DIRECTION('ref_axis',(1.,0.,0.));
#21172=DIRECTION('',(0.,0.,1.));
#21173=DIRECTION('center_axis',(0.279975964635197,0.960007009988256,0.));
#21174=DIRECTION('ref_axis',(0.,0.,1.));
#21175=DIRECTION('',(0.,0.,1.));
#21176=DIRECTION('',(-0.960007009988256,0.279975964635197,0.));
#21177=DIRECTION('',(0.,0.,-1.));
#21178=DIRECTION('center_axis',(0.,0.,1.));
#21179=DIRECTION('ref_axis',(1.,0.,0.));
#21180=DIRECTION('center_axis',(0.,0.,-1.));
#21181=DIRECTION('ref_axis',(1.,0.,0.));
#21182=DIRECTION('center_axis',(0.,0.,1.));
#21183=DIRECTION('ref_axis',(1.,0.,0.));
#21184=DIRECTION('center_axis',(0.,0.,-1.));
#21185=DIRECTION('ref_axis',(1.,0.,0.));
#21186=DIRECTION('center_axis',(0.,0.,1.));
#21187=DIRECTION('ref_axis',(1.,0.,0.));
#21188=DIRECTION('center_axis',(0.,0.,-1.));
#21189=DIRECTION('ref_axis',(1.,0.,0.));
#21190=DIRECTION('center_axis',(0.,0.,1.));
#21191=DIRECTION('ref_axis',(1.,0.,0.));
#21192=DIRECTION('center_axis',(0.,0.,-1.));
#21193=DIRECTION('ref_axis',(1.,0.,0.));
#21194=DIRECTION('center_axis',(0.,0.,1.));
#21195=DIRECTION('ref_axis',(1.,0.,0.));
#21196=DIRECTION('center_axis',(0.,0.,-1.));
#21197=DIRECTION('ref_axis',(1.,0.,0.));
#21198=DIRECTION('center_axis',(0.,0.,1.));
#21199=DIRECTION('ref_axis',(1.,0.,0.));
#21200=DIRECTION('center_axis',(0.,0.,-1.));
#21201=DIRECTION('ref_axis',(1.,0.,0.));
#21202=DIRECTION('center_axis',(0.,0.,1.));
#21203=DIRECTION('ref_axis',(1.,0.,0.));
#21204=DIRECTION('center_axis',(0.,0.,-1.));
#21205=DIRECTION('ref_axis',(1.,0.,0.));
#21206=DIRECTION('center_axis',(0.,0.,1.));
#21207=DIRECTION('ref_axis',(1.,0.,0.));
#21208=DIRECTION('center_axis',(0.,0.,1.));
#21209=DIRECTION('ref_axis',(1.,0.,0.));
#21210=DIRECTION('center_axis',(0.,0.,1.));
#21211=DIRECTION('ref_axis',(1.,0.,0.));
#21212=DIRECTION('center_axis',(0.,0.,1.));
#21213=DIRECTION('ref_axis',(1.,0.,0.));
#21214=DIRECTION('center_axis',(0.,0.,1.));
#21215=DIRECTION('ref_axis',(1.,0.,0.));
#21216=DIRECTION('center_axis',(0.,0.,1.));
#21217=DIRECTION('ref_axis',(1.,0.,0.));
#21218=DIRECTION('center_axis',(0.,0.,1.));
#21219=DIRECTION('ref_axis',(1.,0.,0.));
#21220=DIRECTION('center_axis',(0.,0.,1.));
#21221=DIRECTION('ref_axis',(1.,0.,0.));
#21222=DIRECTION('center_axis',(0.,0.,1.));
#21223=DIRECTION('ref_axis',(1.,0.,0.));
#21224=DIRECTION('center_axis',(0.,0.,1.));
#21225=DIRECTION('ref_axis',(1.,0.,0.));
#21226=DIRECTION('center_axis',(0.,0.,1.));
#21227=DIRECTION('ref_axis',(1.,0.,0.));
#21228=DIRECTION('center_axis',(0.,0.,1.));
#21229=DIRECTION('ref_axis',(1.,0.,0.));
#21230=DIRECTION('center_axis',(0.,0.,1.));
#21231=DIRECTION('ref_axis',(1.,0.,0.));
#21232=DIRECTION('center_axis',(0.,0.,1.));
#21233=DIRECTION('ref_axis',(1.,0.,0.));
#21234=DIRECTION('center_axis',(0.969193219910809,0.246301649362969,0.));
#21235=DIRECTION('ref_axis',(0.,0.,-1.));
#21236=DIRECTION('',(-0.246301649362969,0.969193219910809,0.));
#21237=DIRECTION('',(0.,0.,-1.));
#21238=DIRECTION('center_axis',(0.,0.,-1.));
#21239=DIRECTION('ref_axis',(-0.669130606358858,-0.743144825477394,0.));
#21240=DIRECTION('center_axis',(0.,0.,1.));
#21241=DIRECTION('ref_axis',(-0.669130606358858,-0.743144825477394,0.));
#21242=DIRECTION('center_axis',(0.,0.,1.));
#21243=DIRECTION('ref_axis',(-0.719339800338695,-0.694658370458952,0.));
#21244=DIRECTION('center_axis',(0.,0.,1.));
#21245=DIRECTION('ref_axis',(0.719339800338651,0.694658370458997,0.));
#21246=DIRECTION('center_axis',(0.,0.,1.));
#21247=DIRECTION('ref_axis',(-0.669130606358858,-0.743144825477394,0.));
#21248=DIRECTION('center_axis',(0.,0.,1.));
#21249=DIRECTION('ref_axis',(0.669130606358858,0.743144825477394,0.));
#21250=DIRECTION('center_axis',(0.584125431965383,0.811663402976415,0.));
#21251=DIRECTION('ref_axis',(0.,0.,-1.));
#21252=DIRECTION('',(0.,0.,1.));
#21253=DIRECTION('',(-0.811663402976415,0.584125431965383,0.));
#21254=DIRECTION('',(0.,0.,-1.));
#21255=DIRECTION('center_axis',(0.,0.,-1.));
#21256=DIRECTION('ref_axis',(-0.104528463267653,-0.994521895368273,0.));
#21257=DIRECTION('center_axis',(0.,0.,1.));
#21258=DIRECTION('ref_axis',(-0.104528463267653,-0.994521895368273,0.));
#21259=DIRECTION('center_axis',(0.,0.,1.));
#21260=DIRECTION('ref_axis',(-0.104528463267749,-0.994521895368263,0.));
#21261=DIRECTION('center_axis',(0.,0.,1.));
#21262=DIRECTION('ref_axis',(0.104528463267653,0.994521895368273,0.));
#21263=DIRECTION('',(0.,0.,1.));
#21264=DIRECTION('center_axis',(-0.402606579317095,0.91537311643427,0.));
#21265=DIRECTION('ref_axis',(0.,0.,1.));
#21266=DIRECTION('',(-0.91537311643427,-0.402606579317095,0.));
#21267=DIRECTION('',(0.,0.,-1.));
#21268=DIRECTION('center_axis',(0.639321308629955,0.76893970136265,0.));
#21269=DIRECTION('ref_axis',(0.,0.,-1.));
#21270=DIRECTION('',(0.,0.,1.));
#21271=DIRECTION('',(-0.76893970136265,0.639321308629955,0.));
#21272=DIRECTION('',(0.,0.,-1.));
#21273=DIRECTION('center_axis',(0.,0.,-1.));
#21274=DIRECTION('ref_axis',(-0.17364817766693,-0.984807753012208,0.));
#21275=DIRECTION('center_axis',(0.,0.,1.));
#21276=DIRECTION('ref_axis',(-0.17364817766693,-0.984807753012208,0.));
#21277=DIRECTION('center_axis',(0.,0.,1.));
#21278=DIRECTION('ref_axis',(-0.173648177666931,-0.984807753012208,0.));
#21279=DIRECTION('center_axis',(0.,0.,1.));
#21280=DIRECTION('ref_axis',(0.17364817766693,0.984807753012208,0.));
#21281=DIRECTION('',(0.,0.,1.));
#21282=DIRECTION('center_axis',(-0.337772649161909,0.941227728808574,0.));
#21283=DIRECTION('ref_axis',(0.,0.,1.));
#21284=DIRECTION('',(-0.941227728808574,-0.337772649161909,0.));
#21285=DIRECTION('',(0.,0.,-1.));
#21286=DIRECTION('center_axis',(0.691402476143371,0.722469802817263,0.));
#21287=DIRECTION('ref_axis',(0.,0.,-1.));
#21288=DIRECTION('',(0.,0.,1.));
#21289=DIRECTION('',(-0.722469802817263,0.691402476143371,0.));
#21290=DIRECTION('',(0.,0.,-1.));
#21291=DIRECTION('center_axis',(0.,0.,-1.));
#21292=DIRECTION('ref_axis',(-0.241921895599668,-0.970295726275996,0.));
#21293=DIRECTION('center_axis',(0.,0.,1.));
#21294=DIRECTION('ref_axis',(-0.241921895599668,-0.970295726275996,0.));
#21295=DIRECTION('center_axis',(0.,0.,1.));
#21296=DIRECTION('ref_axis',(-0.241921895599672,-0.970295726275995,0.));
#21297=DIRECTION('center_axis',(0.,0.,1.));
#21298=DIRECTION('ref_axis',(0.241921895599668,0.970295726275996,0.));
#21299=DIRECTION('',(0.,0.,1.));
#21300=DIRECTION('center_axis',(-0.27129312461327,0.962496774299825,0.));
#21301=DIRECTION('ref_axis',(0.,0.,1.));
#21302=DIRECTION('',(-0.962496774299825,-0.27129312461327,0.));
#21303=DIRECTION('',(0.,0.,-1.));
#21304=DIRECTION('center_axis',(0.740115200292261,0.672480104015239,0.));
#21305=DIRECTION('ref_axis',(0.,0.,-1.));
#21306=DIRECTION('',(0.,0.,1.));
#21307=DIRECTION('',(-0.672480104015239,0.740115200292261,0.));
#21308=DIRECTION('',(0.,0.,-1.));
#21309=DIRECTION('center_axis',(0.,0.,-1.));
#21310=DIRECTION('ref_axis',(-0.309016994374948,-0.951056516295154,0.));
#21311=DIRECTION('center_axis',(0.,0.,1.));
#21312=DIRECTION('ref_axis',(-0.309016994374947,-0.951056516295154,0.));
#21313=DIRECTION('center_axis',(0.,0.,1.));
#21314=DIRECTION('ref_axis',(-0.309016994374943,-0.951056516295155,0.));
#21315=DIRECTION('center_axis',(0.,0.,1.));
#21316=DIRECTION('ref_axis',(0.309016994374947,0.951056516295154,0.));
#21317=DIRECTION('',(0.,0.,1.));
#21318=DIRECTION('center_axis',(-0.203491887231385,0.979076632256643,0.));
#21319=DIRECTION('ref_axis',(0.,0.,1.));
#21320=DIRECTION('',(-0.979076632256643,-0.203491887231385,0.));
#21321=DIRECTION('',(0.,0.,-1.));
#21322=DIRECTION('center_axis',(0.785222157581596,0.619214149743772,0.));
#21323=DIRECTION('ref_axis',(0.,0.,-1.));
#21324=DIRECTION('',(0.,0.,1.));
#21325=DIRECTION('',(-0.619214149743772,0.785222157581596,0.));
#21326=DIRECTION('',(0.,0.,-1.));
#21327=DIRECTION('center_axis',(0.,0.,-1.));
#21328=DIRECTION('ref_axis',(-0.374606593415912,-0.927183854566787,0.));
#21329=DIRECTION('center_axis',(0.,0.,1.));
#21330=DIRECTION('ref_axis',(-0.374606593415912,-0.927183854566787,0.));
#21331=DIRECTION('center_axis',(0.,0.,1.));
#21332=DIRECTION('ref_axis',(-0.374606593415899,-0.927183854566793,0.));
#21333=DIRECTION('center_axis',(0.,0.,1.));
#21334=DIRECTION('ref_axis',(0.374606593415912,0.927183854566787,0.));
#21335=DIRECTION('',(0.,0.,1.));
#21336=DIRECTION('center_axis',(-0.134699257830059,0.990886527277484,0.));
#21337=DIRECTION('ref_axis',(0.,0.,1.));
#21338=DIRECTION('',(-0.990886527277484,-0.134699257830059,0.));
#21339=DIRECTION('',(0.,0.,-1.));
#21340=DIRECTION('center_axis',(0.826503591449444,0.56293144637795,0.));
#21341=DIRECTION('ref_axis',(0.,0.,-1.));
#21342=DIRECTION('',(0.,0.,1.));
#21343=DIRECTION('',(-0.56293144637795,0.826503591449444,0.));
#21344=DIRECTION('',(0.,0.,-1.));
#21345=DIRECTION('center_axis',(0.,0.,-1.));
#21346=DIRECTION('ref_axis',(-0.438371146789078,-0.898794046299167,0.));
#21347=DIRECTION('center_axis',(0.,0.,1.));
#21348=DIRECTION('ref_axis',(-0.438371146789077,-0.898794046299167,0.));
#21349=DIRECTION('center_axis',(0.,0.,1.));
#21350=DIRECTION('ref_axis',(-0.438371146789136,-0.898794046299139,0.));
#21351=DIRECTION('center_axis',(0.,0.,1.));
#21352=DIRECTION('ref_axis',(0.438371146789077,0.898794046299167,0.));
#21353=DIRECTION('',(0.,0.,1.));
#21354=DIRECTION('center_axis',(-0.0652503871847199,0.99786892274098,0.));
#21355=DIRECTION('ref_axis',(0.,0.,1.));
#21356=DIRECTION('',(-0.99786892274098,-0.0652503871847199,0.));
#21357=DIRECTION('',(0.,0.,-1.));
#21358=DIRECTION('center_axis',(0.863758382899708,0.503906197590862,0.));
#21359=DIRECTION('ref_axis',(0.,0.,-1.));
#21360=DIRECTION('',(0.,0.,1.));
#21361=DIRECTION('',(-0.503906197590862,0.863758382899708,0.));
#21362=DIRECTION('',(0.,0.,-1.));
#21363=DIRECTION('center_axis',(0.,0.,-1.));
#21364=DIRECTION('ref_axis',(-0.5,-0.866025403784438,0.));
#21365=DIRECTION('center_axis',(0.,0.,1.));
#21366=DIRECTION('ref_axis',(-0.5,-0.866025403784439,0.));
#21367=DIRECTION('center_axis',(0.,0.,1.));
#21368=DIRECTION('ref_axis',(-0.500000000000006,-0.866025403784435,0.));
#21369=DIRECTION('center_axis',(0.,0.,1.));
#21370=DIRECTION('ref_axis',(0.5,0.866025403784439,0.));
#21371=DIRECTION('',(0.,0.,1.));
#21372=DIRECTION('center_axis',(0.0045163767882446,0.999989801118345,0.));
#21373=DIRECTION('ref_axis',(0.,0.,1.));
#21374=DIRECTION('',(-0.999989801118345,0.0045163767882446,0.));
#21375=DIRECTION('',(0.,0.,-1.));
#21376=DIRECTION('center_axis',(0.89680503033297,0.442425968461935,0.));
#21377=DIRECTION('ref_axis',(0.,0.,-1.));
#21378=DIRECTION('',(0.,0.,1.));
#21379=DIRECTION('',(-0.442425968461935,0.89680503033297,0.));
#21380=DIRECTION('',(0.,0.,-1.));
#21381=DIRECTION('center_axis',(0.,0.,-1.));
#21382=DIRECTION('ref_axis',(-0.559192903470747,-0.829037572555042,0.));
#21383=DIRECTION('center_axis',(0.,0.,1.));
#21384=DIRECTION('ref_axis',(-0.559192903470747,-0.829037572555042,0.));
#21385=DIRECTION('center_axis',(0.,0.,1.));
#21386=DIRECTION('ref_axis',(-0.559192903470747,-0.829037572555042,0.));
#21387=DIRECTION('center_axis',(0.,0.,1.));
#21388=DIRECTION('ref_axis',(0.559192903470747,0.829037572555042,0.));
#21389=DIRECTION('',(0.,0.,1.));
#21390=DIRECTION('center_axis',(0.925482533805075,0.378790284486995,0.));
#21391=DIRECTION('ref_axis',(0.,0.,-1.));
#21392=DIRECTION('',(0.,0.,1.));
#21393=DIRECTION('',(-0.378790284486995,0.925482533805075,0.));
#21394=DIRECTION('',(0.,0.,-1.));
#21395=DIRECTION('center_axis',(0.,0.,1.));
#21396=DIRECTION('ref_axis',(1.,0.,0.));
#21397=DIRECTION('center_axis',(0.,0.,-1.));
#21398=DIRECTION('ref_axis',(1.,0.,0.));
#21399=DIRECTION('',(0.,0.,-1.));
#21400=DIRECTION('center_axis',(0.,0.,1.));
#21401=DIRECTION('ref_axis',(1.,0.,0.));
#21402=DIRECTION('center_axis',(0.,0.,1.));
#21403=DIRECTION('ref_axis',(1.,0.,0.));
#21404=DIRECTION('center_axis',(0.0742611374276901,0.997238829703269,0.));
#21405=DIRECTION('ref_axis',(0.,0.,1.));
#21406=DIRECTION('',(-0.997238829703269,0.0742611374276901,0.));
#21407=DIRECTION('center_axis',(-0.526083754912358,0.850432762078998,0.));
#21408=DIRECTION('ref_axis',(0.,0.,1.));
#21409=DIRECTION('',(-0.850432762078998,-0.526083754912358,0.));
#21410=DIRECTION('',(0.,0.,-1.));
#21411=DIRECTION('',(0.,0.,1.));
#21412=DIRECTION('center_axis',(0.,0.,1.));
#21413=DIRECTION('ref_axis',(1.,0.,0.));
#21414=DIRECTION('center_axis',(0.,0.,-1.));
#21415=DIRECTION('ref_axis',(1.,0.,0.));
#21416=DIRECTION('center_axis',(0.,0.,1.));
#21417=DIRECTION('ref_axis',(1.,0.,0.));
#21418=DIRECTION('center_axis',(0.,0.,1.));
#21419=DIRECTION('ref_axis',(1.,0.,0.));
#21420=DIRECTION('',(0.,0.,1.));
#21421=DIRECTION('center_axis',(-0.465479050687347,0.885058898249832,0.));
#21422=DIRECTION('ref_axis',(0.,0.,1.));
#21423=DIRECTION('',(0.,0.,1.));
#21424=DIRECTION('',(-0.885058898249832,-0.465479050687346,0.));
#21425=DIRECTION('',(0.,0.,-1.));
#21426=DIRECTION('center_axis',(0.,0.,1.));
#21427=DIRECTION('ref_axis',(1.,0.,0.));
#21428=DIRECTION('center_axis',(0.,0.,-1.));
#21429=DIRECTION('ref_axis',(1.,0.,0.));
#21430=DIRECTION('center_axis',(0.,0.,1.));
#21431=DIRECTION('ref_axis',(1.,0.,0.));
#21432=DIRECTION('center_axis',(0.,0.,-1.));
#21433=DIRECTION('ref_axis',(1.,0.,0.));
#21434=DIRECTION('center_axis',(0.,0.,1.));
#21435=DIRECTION('ref_axis',(1.,0.,0.));
#21436=DIRECTION('center_axis',(0.,0.,-1.));
#21437=DIRECTION('ref_axis',(1.,0.,0.));
#21438=DIRECTION('center_axis',(0.,0.,1.));
#21439=DIRECTION('ref_axis',(1.,0.,0.));
#21440=DIRECTION('center_axis',(0.,0.,-1.));
#21441=DIRECTION('ref_axis',(1.,0.,0.));
#21442=DIRECTION('center_axis',(0.,0.,1.));
#21443=DIRECTION('ref_axis',(1.,0.,0.));
#21444=DIRECTION('center_axis',(0.,0.,-1.));
#21445=DIRECTION('ref_axis',(1.,0.,0.));
#21446=DIRECTION('center_axis',(0.,0.,1.));
#21447=DIRECTION('ref_axis',(1.,0.,0.));
#21448=DIRECTION('center_axis',(0.,0.,-1.));
#21449=DIRECTION('ref_axis',(1.,0.,0.));
#21450=DIRECTION('center_axis',(0.,0.,1.));
#21451=DIRECTION('ref_axis',(1.,0.,0.));
#21452=DIRECTION('center_axis',(0.,0.,-1.));
#21453=DIRECTION('ref_axis',(1.,0.,0.));
#21454=DIRECTION('center_axis',(0.,0.,1.));
#21455=DIRECTION('ref_axis',(1.,0.,0.));
#21456=DIRECTION('center_axis',(0.,0.,-1.));
#21457=DIRECTION('ref_axis',(1.,0.,0.));
#21458=DIRECTION('center_axis',(0.,0.,1.));
#21459=DIRECTION('ref_axis',(1.,0.,0.));
#21460=DIRECTION('center_axis',(0.,0.,1.));
#21461=DIRECTION('ref_axis',(1.,0.,0.));
#21462=DIRECTION('center_axis',(0.,0.,1.));
#21463=DIRECTION('ref_axis',(1.,0.,0.));
#21464=DIRECTION('center_axis',(0.,0.,1.));
#21465=DIRECTION('ref_axis',(1.,0.,0.));
#21466=DIRECTION('center_axis',(0.,0.,1.));
#21467=DIRECTION('ref_axis',(1.,0.,0.));
#21468=DIRECTION('center_axis',(0.,0.,1.));
#21469=DIRECTION('ref_axis',(1.,0.,0.));
#21470=DIRECTION('center_axis',(0.,0.,1.));
#21471=DIRECTION('ref_axis',(1.,0.,0.));
#21472=DIRECTION('center_axis',(0.,0.,1.));
#21473=DIRECTION('ref_axis',(1.,0.,0.));
#21474=DIRECTION('center_axis',(0.,0.,1.));
#21475=DIRECTION('ref_axis',(1.,0.,0.));
#21476=DIRECTION('center_axis',(0.,0.,1.));
#21477=DIRECTION('ref_axis',(1.,0.,0.));
#21478=DIRECTION('center_axis',(0.,0.,1.));
#21479=DIRECTION('ref_axis',(1.,0.,0.));
#21480=DIRECTION('center_axis',(0.,0.,1.));
#21481=DIRECTION('ref_axis',(1.,0.,0.));
#21482=DIRECTION('center_axis',(0.,0.,1.));
#21483=DIRECTION('ref_axis',(1.,0.,0.));
#21484=DIRECTION('center_axis',(0.,0.,1.));
#21485=DIRECTION('ref_axis',(1.,0.,0.));
#21486=DIRECTION('center_axis',(0.,0.,1.));
#21487=DIRECTION('ref_axis',(1.,0.,0.));
#21488=DIRECTION('center_axis',(0.,0.,1.));
#21489=DIRECTION('ref_axis',(1.,0.,0.));
#21490=DIRECTION('center_axis',(0.526083754912358,0.850432762078998,0.));
#21491=DIRECTION('ref_axis',(0.,0.,-1.));
#21492=DIRECTION('',(-0.850432762078998,0.526083754912358,0.));
#21493=DIRECTION('',(0.,0.,-1.));
#21494=DIRECTION('center_axis',(0.,0.,1.));
#21495=DIRECTION('ref_axis',(-0.0348994967025649,-0.999390827019094,0.));
#21496=DIRECTION('center_axis',(0.,0.,1.));
#21497=DIRECTION('ref_axis',(0.0348994967025011,0.999390827019096,0.));
#21498=DIRECTION('center_axis',(-0.949651179401728,0.313309172321697,0.));
#21499=DIRECTION('ref_axis',(0.,0.,1.));
#21500=DIRECTION('',(-0.313309172321697,-0.949651179401728,0.));
#21501=DIRECTION('',(0.,0.,-1.));
#21502=DIRECTION('',(0.,0.,1.));
#21503=DIRECTION('center_axis',(0.,0.,1.));
#21504=DIRECTION('ref_axis',(-1.,0.,0.));
#21505=DIRECTION('center_axis',(0.,0.,-1.));
#21506=DIRECTION('ref_axis',(-1.,0.,0.));
#21507=DIRECTION('center_axis',(0.,0.,1.));
#21508=DIRECTION('ref_axis',(1.,0.,0.));
#21509=DIRECTION('center_axis',(0.,0.,1.));
#21510=DIRECTION('ref_axis',(1.,0.,0.));
#21511=DIRECTION('',(0.,0.,1.));
#21512=DIRECTION('center_axis',(-0.143644105269892,0.989629410952005,0.));
#21513=DIRECTION('ref_axis',(0.,0.,1.));
#21514=DIRECTION('',(-0.989629410952005,-0.143644105269892,0.));
#21515=DIRECTION('',(0.,0.,-1.));
#21516=DIRECTION('center_axis',(-0.925482533805075,0.378790284486995,0.));
#21517=DIRECTION('ref_axis',(0.,0.,1.));
#21518=DIRECTION('',(-0.378790284486995,-0.925482533805075,0.));
#21519=DIRECTION('',(0.,0.,-1.));
#21520=DIRECTION('',(0.,0.,1.));
#21521=DIRECTION('center_axis',(0.,0.,1.));
#21522=DIRECTION('ref_axis',(-1.,0.,0.));
#21523=DIRECTION('center_axis',(0.,0.,-1.));
#21524=DIRECTION('ref_axis',(-1.,0.,0.));
#21525=DIRECTION('center_axis',(0.,0.,1.));
#21526=DIRECTION('ref_axis',(1.,0.,0.));
#21527=DIRECTION('center_axis',(0.,0.,1.));
#21528=DIRECTION('ref_axis',(1.,0.,0.));
#21529=DIRECTION('',(0.,0.,1.));
#21530=DIRECTION('center_axis',(-0.0742611374276901,0.997238829703269,0.));
#21531=DIRECTION('ref_axis',(0.,0.,1.));
#21532=DIRECTION('',(-0.997238829703269,-0.0742611374276901,0.));
#21533=DIRECTION('',(0.,0.,-1.));
#21534=DIRECTION('center_axis',(-0.89680503033297,0.442425968461935,0.));
#21535=DIRECTION('ref_axis',(0.,0.,1.));
#21536=DIRECTION('',(-0.442425968461935,-0.89680503033297,0.));
#21537=DIRECTION('',(0.,0.,-1.));
#21538=DIRECTION('',(0.,0.,1.));
#21539=DIRECTION('center_axis',(0.,0.,1.));
#21540=DIRECTION('ref_axis',(-1.,0.,0.));
#21541=DIRECTION('center_axis',(0.,0.,-1.));
#21542=DIRECTION('ref_axis',(-1.,0.,0.));
#21543=DIRECTION('center_axis',(0.,0.,1.));
#21544=DIRECTION('ref_axis',(1.,0.,0.));
#21545=DIRECTION('center_axis',(0.,0.,1.));
#21546=DIRECTION('ref_axis',(1.,0.,0.));
#21547=DIRECTION('',(0.,0.,1.));
#21548=DIRECTION('center_axis',(-0.0045163767882446,0.999989801118345,0.));
#21549=DIRECTION('ref_axis',(0.,0.,1.));
#21550=DIRECTION('',(-0.999989801118345,-0.0045163767882446,0.));
#21551=DIRECTION('',(0.,0.,-1.));
#21552=DIRECTION('center_axis',(-0.863758382899608,0.503906197591034,0.));
#21553=DIRECTION('ref_axis',(0.,0.,1.));
#21554=DIRECTION('',(-0.503906197591034,-0.863758382899608,0.));
#21555=DIRECTION('',(0.,0.,-1.));
#21556=DIRECTION('',(0.,0.,1.));
#21557=DIRECTION('center_axis',(0.,0.,1.));
#21558=DIRECTION('ref_axis',(-1.,0.,0.));
#21559=DIRECTION('center_axis',(0.,0.,-1.));
#21560=DIRECTION('ref_axis',(-1.,0.,0.));
#21561=DIRECTION('center_axis',(0.,0.,1.));
#21562=DIRECTION('ref_axis',(1.,0.,0.));
#21563=DIRECTION('center_axis',(0.,0.,1.));
#21564=DIRECTION('ref_axis',(1.,0.,0.));
#21565=DIRECTION('',(0.,0.,1.));
#21566=DIRECTION('center_axis',(0.065250387184499,0.997868922740995,0.));
#21567=DIRECTION('ref_axis',(0.,0.,1.));
#21568=DIRECTION('',(-0.997868922740995,0.065250387184499,0.));
#21569=DIRECTION('',(0.,0.,-1.));
#21570=DIRECTION('center_axis',(-0.826503591449438,0.562931446377958,0.));
#21571=DIRECTION('ref_axis',(0.,0.,1.));
#21572=DIRECTION('',(-0.562931446377958,-0.826503591449438,0.));
#21573=DIRECTION('',(0.,0.,-1.));
#21574=DIRECTION('',(0.,0.,1.));
#21575=DIRECTION('center_axis',(0.,0.,1.));
#21576=DIRECTION('ref_axis',(-1.,0.,0.));
#21577=DIRECTION('center_axis',(0.,0.,-1.));
#21578=DIRECTION('ref_axis',(-1.,0.,0.));
#21579=DIRECTION('center_axis',(0.,0.,1.));
#21580=DIRECTION('ref_axis',(1.,0.,0.));
#21581=DIRECTION('center_axis',(0.,0.,1.));
#21582=DIRECTION('ref_axis',(1.,0.,0.));
#21583=DIRECTION('',(0.,0.,1.));
#21584=DIRECTION('center_axis',(0.134699257830059,0.990886527277484,0.));
#21585=DIRECTION('ref_axis',(0.,0.,1.));
#21586=DIRECTION('',(-0.990886527277484,0.134699257830059,0.));
#21587=DIRECTION('',(0.,0.,-1.));
#21588=DIRECTION('center_axis',(-0.785222157581596,0.619214149743772,0.));
#21589=DIRECTION('ref_axis',(0.,0.,1.));
#21590=DIRECTION('',(-0.619214149743772,-0.785222157581596,0.));
#21591=DIRECTION('',(0.,0.,-1.));
#21592=DIRECTION('',(0.,0.,1.));
#21593=DIRECTION('center_axis',(0.,0.,1.));
#21594=DIRECTION('ref_axis',(-1.,0.,0.));
#21595=DIRECTION('center_axis',(0.,0.,-1.));
#21596=DIRECTION('ref_axis',(-1.,0.,0.));
#21597=DIRECTION('center_axis',(0.,0.,1.));
#21598=DIRECTION('ref_axis',(1.,0.,0.));
#21599=DIRECTION('center_axis',(0.,0.,1.));
#21600=DIRECTION('ref_axis',(1.,0.,0.));
#21601=DIRECTION('',(0.,0.,1.));
#21602=DIRECTION('center_axis',(0.203491887231601,0.979076632256598,0.));
#21603=DIRECTION('ref_axis',(0.,0.,1.));
#21604=DIRECTION('',(-0.979076632256598,0.203491887231601,0.));
#21605=DIRECTION('',(0.,0.,-1.));
#21606=DIRECTION('center_axis',(-0.740115200292264,0.672480104015236,0.));
#21607=DIRECTION('ref_axis',(0.,0.,1.));
#21608=DIRECTION('',(-0.672480104015236,-0.740115200292264,0.));
#21609=DIRECTION('',(0.,0.,-1.));
#21610=DIRECTION('',(0.,0.,1.));
#21611=DIRECTION('center_axis',(0.,0.,1.));
#21612=DIRECTION('ref_axis',(-1.,0.,0.));
#21613=DIRECTION('center_axis',(0.,0.,-1.));
#21614=DIRECTION('ref_axis',(-1.,0.,0.));
#21615=DIRECTION('center_axis',(0.,0.,1.));
#21616=DIRECTION('ref_axis',(1.,0.,0.));
#21617=DIRECTION('center_axis',(0.,0.,1.));
#21618=DIRECTION('ref_axis',(1.,0.,0.));
#21619=DIRECTION('',(0.,0.,1.));
#21620=DIRECTION('center_axis',(0.271293124613069,0.962496774299882,0.));
#21621=DIRECTION('ref_axis',(0.,0.,1.));
#21622=DIRECTION('',(-0.962496774299882,0.271293124613069,0.));
#21623=DIRECTION('',(0.,0.,-1.));
#21624=DIRECTION('center_axis',(-0.691402476143223,0.722469802817405,0.));
#21625=DIRECTION('ref_axis',(0.,0.,1.));
#21626=DIRECTION('',(-0.722469802817405,-0.691402476143223,0.));
#21627=DIRECTION('',(0.,0.,-1.));
#21628=DIRECTION('',(0.,0.,1.));
#21629=DIRECTION('center_axis',(0.,0.,1.));
#21630=DIRECTION('ref_axis',(-1.,0.,0.));
#21631=DIRECTION('center_axis',(0.,0.,-1.));
#21632=DIRECTION('ref_axis',(-1.,0.,0.));
#21633=DIRECTION('center_axis',(0.,0.,1.));
#21634=DIRECTION('ref_axis',(1.,0.,0.));
#21635=DIRECTION('center_axis',(0.,0.,1.));
#21636=DIRECTION('ref_axis',(1.,0.,0.));
#21637=DIRECTION('',(0.,0.,1.));
#21638=DIRECTION('center_axis',(0.337772649161909,0.941227728808574,0.));
#21639=DIRECTION('ref_axis',(0.,0.,1.));
#21640=DIRECTION('',(-0.941227728808574,0.337772649161909,0.));
#21641=DIRECTION('',(0.,0.,-1.));
#21642=DIRECTION('center_axis',(-0.639321308629956,0.768939701362649,0.));
#21643=DIRECTION('ref_axis',(0.,0.,1.));
#21644=DIRECTION('',(-0.768939701362649,-0.639321308629956,0.));
#21645=DIRECTION('',(0.,0.,-1.));
#21646=DIRECTION('',(0.,0.,1.));
#21647=DIRECTION('center_axis',(0.,0.,1.));
#21648=DIRECTION('ref_axis',(-1.,0.,0.));
#21649=DIRECTION('center_axis',(0.,0.,-1.));
#21650=DIRECTION('ref_axis',(-1.,0.,0.));
#21651=DIRECTION('center_axis',(0.,0.,1.));
#21652=DIRECTION('ref_axis',(1.,0.,0.));
#21653=DIRECTION('center_axis',(0.,0.,1.));
#21654=DIRECTION('ref_axis',(1.,0.,0.));
#21655=DIRECTION('',(0.,0.,1.));
#21656=DIRECTION('center_axis',(-0.584125431965383,0.811663402976415,0.));
#21657=DIRECTION('ref_axis',(0.,0.,1.));
#21658=DIRECTION('',(-0.811663402976415,-0.584125431965383,0.));
#21659=DIRECTION('',(0.,0.,1.));
#21660=DIRECTION('center_axis',(0.,0.,1.));
#21661=DIRECTION('ref_axis',(0.104528463267749,-0.994521895368263,0.));
#21662=DIRECTION('center_axis',(0.,0.,1.));
#21663=DIRECTION('ref_axis',(0.104528463267654,-0.994521895368273,0.));
#21664=DIRECTION('',(0.,0.,-1.));
#21665=DIRECTION('center_axis',(0.,0.,1.));
#21666=DIRECTION('ref_axis',(-0.104528463267654,0.994521895368273,0.));
#21667=DIRECTION('center_axis',(0.,0.,-1.));
#21668=DIRECTION('ref_axis',(0.104528463267654,-0.994521895368273,0.));
#21669=DIRECTION('center_axis',(0.402606579317095,0.91537311643427,0.));
#21670=DIRECTION('ref_axis',(0.,0.,1.));
#21671=DIRECTION('',(-0.91537311643427,0.402606579317095,0.));
#21672=DIRECTION('center_axis',(0.,0.,-1.));
#21673=DIRECTION('ref_axis',(0.615661475325658,-0.788010753606722,0.));
#21674=DIRECTION('center_axis',(0.,0.,1.));
#21675=DIRECTION('ref_axis',(0.615661475325658,-0.788010753606722,0.));
#21676=DIRECTION('center_axis',(0.,0.,-1.));
#21677=DIRECTION('ref_axis',(0.559192903470747,-0.829037572555042,0.));
#21678=DIRECTION('center_axis',(0.,0.,1.));
#21679=DIRECTION('ref_axis',(0.559192903470747,-0.829037572555042,0.));
#21680=DIRECTION('center_axis',(0.,0.,-1.));
#21681=DIRECTION('ref_axis',(0.5,-0.866025403784439,0.));
#21682=DIRECTION('center_axis',(0.,0.,1.));
#21683=DIRECTION('ref_axis',(0.5,-0.866025403784439,0.));
#21684=DIRECTION('center_axis',(0.,0.,-1.));
#21685=DIRECTION('ref_axis',(0.438371146789078,-0.898794046299167,0.));
#21686=DIRECTION('center_axis',(0.,0.,1.));
#21687=DIRECTION('ref_axis',(0.438371146789078,-0.898794046299167,0.));
#21688=DIRECTION('center_axis',(0.,0.,-1.));
#21689=DIRECTION('ref_axis',(0.374606593415912,-0.927183854566787,0.));
#21690=DIRECTION('center_axis',(0.,0.,1.));
#21691=DIRECTION('ref_axis',(0.374606593415912,-0.927183854566787,0.));
#21692=DIRECTION('center_axis',(0.,0.,-1.));
#21693=DIRECTION('ref_axis',(0.309016994374947,-0.951056516295154,0.));
#21694=DIRECTION('center_axis',(0.,0.,1.));
#21695=DIRECTION('ref_axis',(0.309016994374947,-0.951056516295154,0.));
#21696=DIRECTION('center_axis',(0.,0.,-1.));
#21697=DIRECTION('ref_axis',(0.241921895599668,-0.970295726275996,0.));
#21698=DIRECTION('center_axis',(0.,0.,1.));
#21699=DIRECTION('ref_axis',(0.241921895599668,-0.970295726275996,0.));
#21700=DIRECTION('center_axis',(0.,0.,-1.));
#21701=DIRECTION('ref_axis',(0.17364817766693,-0.984807753012208,0.));
#21702=DIRECTION('center_axis',(0.,0.,1.));
#21703=DIRECTION('ref_axis',(0.17364817766693,-0.984807753012208,0.));
#21704=DIRECTION('center_axis',(0.,0.,1.));
#21705=DIRECTION('ref_axis',(0.173648177666931,-0.984807753012208,0.));
#21706=DIRECTION('center_axis',(0.,0.,1.));
#21707=DIRECTION('ref_axis',(-0.17364817766693,0.984807753012208,0.));
#21708=DIRECTION('center_axis',(0.,0.,1.));
#21709=DIRECTION('ref_axis',(0.241921895599671,-0.970295726275996,0.));
#21710=DIRECTION('center_axis',(0.,0.,1.));
#21711=DIRECTION('ref_axis',(-0.241921895599668,0.970295726275996,0.));
#21712=DIRECTION('center_axis',(0.,0.,1.));
#21713=DIRECTION('ref_axis',(0.309016994374995,-0.951056516295138,0.));
#21714=DIRECTION('center_axis',(0.,0.,1.));
#21715=DIRECTION('ref_axis',(-0.309016994374947,0.951056516295154,0.));
#21716=DIRECTION('center_axis',(0.,0.,1.));
#21717=DIRECTION('ref_axis',(0.374606593415899,-0.927183854566793,0.));
#21718=DIRECTION('center_axis',(0.,0.,1.));
#21719=DIRECTION('ref_axis',(-0.374606593415912,0.927183854566787,0.));
#21720=DIRECTION('center_axis',(0.,0.,1.));
#21721=DIRECTION('ref_axis',(0.438371146789079,-0.898794046299166,0.));
#21722=DIRECTION('center_axis',(0.,0.,1.));
#21723=DIRECTION('ref_axis',(-0.438371146789078,0.898794046299167,0.));
#21724=DIRECTION('center_axis',(0.,0.,1.));
#21725=DIRECTION('ref_axis',(0.500000000000058,-0.866025403784405,0.));
#21726=DIRECTION('center_axis',(0.,0.,1.));
#21727=DIRECTION('ref_axis',(-0.5,0.866025403784439,0.));
#21728=DIRECTION('center_axis',(0.,0.,1.));
#21729=DIRECTION('ref_axis',(0.559192903470747,-0.829037572555042,0.));
#21730=DIRECTION('center_axis',(0.,0.,1.));
#21731=DIRECTION('ref_axis',(-0.559192903470747,0.829037572555042,0.));
#21732=DIRECTION('center_axis',(0.,0.,1.));
#21733=DIRECTION('ref_axis',(0.615661475325708,-0.788010753606683,0.));
#21734=DIRECTION('center_axis',(0.,0.,1.));
#21735=DIRECTION('ref_axis',(-0.615661475325658,0.788010753606722,0.));
#21736=DIRECTION('center_axis',(0.,0.,-1.));
#21737=DIRECTION('ref_axis',(1.,0.,0.));
#21738=DIRECTION('center_axis',(0.,0.,1.));
#21739=DIRECTION('ref_axis',(1.,0.,0.));
#21740=DIRECTION('',(-0.707106781186546,-8.65956056235491E-17,-0.707106781186549));
#21741=DIRECTION('center_axis',(0.,0.,1.));
#21742=DIRECTION('ref_axis',(1.,0.,0.));
#21743=DIRECTION('center_axis',(0.,0.,-1.));
#21744=DIRECTION('ref_axis',(1.,0.,0.));
#21745=DIRECTION('',(0.,0.,-1.));
#21746=DIRECTION('center_axis',(-0.952442453762929,-0.304718513172487,0.));
#21747=DIRECTION('ref_axis',(0.,0.,1.));
#21748=DIRECTION('',(0.,0.,1.));
#21749=DIRECTION('',(0.304718513172487,-0.952442453762929,0.));
#21750=DIRECTION('center_axis',(0.,0.,-1.));
#21751=DIRECTION('ref_axis',(0.961261695938319,-0.275637355816999,0.));
#21752=DIRECTION('center_axis',(0.,0.,1.));
#21753=DIRECTION('ref_axis',(0.961261695938319,-0.275637355816999,0.));
#21754=DIRECTION('center_axis',(0.,0.,-1.));
#21755=DIRECTION('ref_axis',(0.939692620785908,-0.342020143325669,0.));
#21756=DIRECTION('center_axis',(0.,0.,1.));
#21757=DIRECTION('ref_axis',(0.939692620785908,-0.342020143325669,0.));
#21758=DIRECTION('center_axis',(0.,0.,-1.));
#21759=DIRECTION('ref_axis',(0.913545457642601,-0.4067366430758,0.));
#21760=DIRECTION('center_axis',(0.,0.,1.));
#21761=DIRECTION('ref_axis',(0.913545457642601,-0.4067366430758,0.));
#21762=DIRECTION('center_axis',(0.,0.,-1.));
#21763=DIRECTION('ref_axis',(0.882947592858927,-0.469471562785891,0.));
#21764=DIRECTION('center_axis',(0.,0.,1.));
#21765=DIRECTION('ref_axis',(0.882947592858927,-0.469471562785891,0.));
#21766=DIRECTION('center_axis',(0.,0.,-1.));
#21767=DIRECTION('ref_axis',(0.848048096156426,-0.529919264233205,0.));
#21768=DIRECTION('center_axis',(0.,0.,1.));
#21769=DIRECTION('ref_axis',(0.848048096156426,-0.529919264233205,0.));
#21770=DIRECTION('center_axis',(0.,0.,-1.));
#21771=DIRECTION('ref_axis',(0.809016994374947,-0.587785252292473,0.));
#21772=DIRECTION('center_axis',(0.,0.,1.));
#21773=DIRECTION('ref_axis',(0.809016994374947,-0.587785252292473,0.));
#21774=DIRECTION('center_axis',(0.,0.,-1.));
#21775=DIRECTION('ref_axis',(0.766044443118978,-0.642787609686539,0.));
#21776=DIRECTION('center_axis',(0.,0.,1.));
#21777=DIRECTION('ref_axis',(0.766044443118978,-0.642787609686539,0.));
#21778=DIRECTION('center_axis',(0.,0.,-1.));
#21779=DIRECTION('ref_axis',(0.719339800338651,-0.694658370458997,0.));
#21780=DIRECTION('center_axis',(0.,0.,1.));
#21781=DIRECTION('ref_axis',(0.719339800338651,-0.694658370458997,0.));
#21782=DIRECTION('center_axis',(0.,0.,1.));
#21783=DIRECTION('ref_axis',(0.669130606358858,-0.743144825477395,0.));
#21784=DIRECTION('center_axis',(0.,0.,1.));
#21785=DIRECTION('ref_axis',(-0.669130606358858,0.743144825477394,0.));
#21786=DIRECTION('center_axis',(0.,0.,1.));
#21787=DIRECTION('ref_axis',(0.719339800338695,-0.694658370458952,0.));
#21788=DIRECTION('center_axis',(0.,0.,1.));
#21789=DIRECTION('ref_axis',(-0.719339800338651,0.694658370458997,0.));
#21790=DIRECTION('center_axis',(0.,0.,1.));
#21791=DIRECTION('ref_axis',(0.76604444311897,-0.642787609686549,0.));
#21792=DIRECTION('center_axis',(0.,0.,1.));
#21793=DIRECTION('ref_axis',(-0.766044443118978,0.642787609686539,0.));
#21794=DIRECTION('center_axis',(0.,0.,1.));
#21795=DIRECTION('ref_axis',(0.809016994374945,-0.587785252292477,0.));
#21796=DIRECTION('center_axis',(0.,0.,1.));
#21797=DIRECTION('ref_axis',(-0.809016994374947,0.587785252292473,0.));
#21798=DIRECTION('center_axis',(0.,0.,1.));
#21799=DIRECTION('ref_axis',(0.848048096156423,-0.52991926423321,0.));
#21800=DIRECTION('center_axis',(0.,0.,1.));
#21801=DIRECTION('ref_axis',(-0.848048096156426,0.529919264233205,0.));
#21802=DIRECTION('center_axis',(0.,0.,1.));
#21803=DIRECTION('ref_axis',(0.882947592858954,-0.469471562785839,0.));
#21804=DIRECTION('center_axis',(0.,0.,1.));
#21805=DIRECTION('ref_axis',(-0.882947592858927,0.469471562785891,0.));
#21806=DIRECTION('center_axis',(0.,0.,1.));
#21807=DIRECTION('ref_axis',(0.913545457642601,-0.406736643075801,0.));
#21808=DIRECTION('center_axis',(0.,0.,1.));
#21809=DIRECTION('ref_axis',(-0.913545457642601,0.4067366430758,0.));
#21810=DIRECTION('center_axis',(0.,0.,1.));
#21811=DIRECTION('ref_axis',(0.939692620785906,-0.342020143325675,0.));
#21812=DIRECTION('center_axis',(0.,0.,1.));
#21813=DIRECTION('ref_axis',(-0.939692620785908,0.342020143325669,0.));
#21814=DIRECTION('center_axis',(0.,0.,1.));
#21815=DIRECTION('ref_axis',(0.96126169593832,-0.275637355816994,0.));
#21816=DIRECTION('center_axis',(0.,0.,1.));
#21817=DIRECTION('ref_axis',(-0.961261695938319,0.275637355816999,0.));
#21818=DIRECTION('center_axis',(-0.746159292170122,0.665767459934911,0.));
#21819=DIRECTION('ref_axis',(0.,0.,1.));
#21820=DIRECTION('',(0.,0.,1.));
#21821=DIRECTION('',(-0.665767459934911,-0.746159292170122,0.));
#21822=DIRECTION('',(0.,0.,-1.));
#21823=DIRECTION('center_axis',(0.,0.,1.));
#21824=DIRECTION('ref_axis',(0.978147600733817,-0.207911690817704,0.));
#21825=DIRECTION('center_axis',(0.,0.,1.));
#21826=DIRECTION('ref_axis',(-0.978147600733806,0.207911690817759,0.));
#21827=DIRECTION('center_axis',(-0.697900095297744,-0.716195124936913,0.));
#21828=DIRECTION('ref_axis',(0.,0.,1.));
#21829=DIRECTION('',(0.716195124936913,-0.697900095297744,0.));
#21830=DIRECTION('',(0.,0.,-1.));
#21831=DIRECTION('center_axis',(0.,0.,1.));
#21832=DIRECTION('ref_axis',(-1.,0.,0.));
#21833=DIRECTION('center_axis',(0.,0.,-1.));
#21834=DIRECTION('ref_axis',(-1.,0.,0.));
#21835=DIRECTION('center_axis',(-0.952442453762929,0.304718513172488,0.));
#21836=DIRECTION('ref_axis',(0.,0.,1.));
#21837=DIRECTION('',(0.,0.,1.));
#21838=DIRECTION('',(-0.304718513172488,-0.952442453762928,0.));
#21839=DIRECTION('',(0.,0.,-1.));
#21840=DIRECTION('center_axis',(0.,0.,1.));
#21841=DIRECTION('ref_axis',(0.978147600733804,0.207911690817768,0.));
#21842=DIRECTION('center_axis',(0.,0.,1.));
#21843=DIRECTION('ref_axis',(-0.978147600733806,-0.20791169081776,0.));
#21844=DIRECTION('',(0.,0.,1.));
#21845=DIRECTION('center_axis',(-0.900764728877144,-0.43430738332532,0.));
#21846=DIRECTION('ref_axis',(0.,0.,1.));
#21847=DIRECTION('',(0.,0.,1.));
#21848=DIRECTION('',(0.43430738332532,-0.900764728877144,0.));
#21849=DIRECTION('',(0.,0.,-1.));
#21850=DIRECTION('center_axis',(0.,0.,1.));
#21851=DIRECTION('ref_axis',(-1.,0.,0.));
#21852=DIRECTION('center_axis',(0.,0.,-1.));
#21853=DIRECTION('ref_axis',(-1.,0.,0.));
#21854=DIRECTION('center_axis',(-0.790783275974884,0.61209624279065,0.));
#21855=DIRECTION('ref_axis',(0.,0.,1.));
#21856=DIRECTION('',(0.,0.,1.));
#21857=DIRECTION('',(-0.61209624279065,-0.790783275974884,0.));
#21858=DIRECTION('center_axis',(0.,0.,1.));
#21859=DIRECTION('ref_axis',(0.997564050259824,-0.0697564737441227,0.));
#21860=DIRECTION('',(0.,0.,-1.));
#21861=DIRECTION('center_axis',(0.,0.,1.));
#21862=DIRECTION('ref_axis',(-0.997564050259824,0.0697564737441255,0.));
#21863=DIRECTION('center_axis',(-0.746159292170273,-0.665767459934741,0.));
#21864=DIRECTION('ref_axis',(0.,0.,1.));
#21865=DIRECTION('',(0.665767459934741,-0.746159292170273,0.));
#21866=DIRECTION('',(0.,0.,-1.));
#21867=DIRECTION('center_axis',(0.,0.,1.));
#21868=DIRECTION('ref_axis',(-1.,0.,0.));
#21869=DIRECTION('center_axis',(0.,0.,-1.));
#21870=DIRECTION('ref_axis',(-1.,0.,0.));
#21871=DIRECTION('center_axis',(-0.92886626285169,0.370415261208196,0.));
#21872=DIRECTION('ref_axis',(0.,0.,1.));
#21873=DIRECTION('',(0.,0.,1.));
#21874=DIRECTION('',(-0.370415261208196,-0.928866262851689,0.));
#21875=DIRECTION('',(0.,0.,-1.));
#21876=DIRECTION('center_axis',(0.,0.,1.));
#21877=DIRECTION('ref_axis',(0.99026806874158,0.139173100959998,0.));
#21878=DIRECTION('center_axis',(0.,0.,1.));
#21879=DIRECTION('ref_axis',(-0.99026806874157,-0.139173100960066,0.));
#21880=DIRECTION('',(0.,0.,1.));
#21881=DIRECTION('center_axis',(-0.868274759687958,-0.496083603527489,0.));
#21882=DIRECTION('ref_axis',(0.,0.,1.));
#21883=DIRECTION('',(0.,0.,1.));
#21884=DIRECTION('',(0.496083603527489,-0.868274759687958,0.));
#21885=DIRECTION('',(0.,0.,-1.));
#21886=DIRECTION('center_axis',(0.,0.,1.));
#21887=DIRECTION('ref_axis',(-1.,0.,0.));
#21888=DIRECTION('center_axis',(0.,0.,-1.));
#21889=DIRECTION('ref_axis',(-1.,0.,0.));
#21890=DIRECTION('center_axis',(-0.831554643148455,0.555442954279056,0.));
#21891=DIRECTION('ref_axis',(0.,0.,1.));
#21892=DIRECTION('',(0.,0.,1.));
#21893=DIRECTION('',(-0.555442954279056,-0.831554643148455,0.));
#21894=DIRECTION('center_axis',(0.,0.,1.));
#21895=DIRECTION('ref_axis',(1.,0.,0.));
#21896=DIRECTION('',(0.,0.,-1.));
#21897=DIRECTION('center_axis',(0.,0.,1.));
#21898=DIRECTION('ref_axis',(-1.,1.22464679914735E-16,0.));
#21899=DIRECTION('center_axis',(-0.790783275974884,-0.61209624279065,0.));
#21900=DIRECTION('ref_axis',(0.,0.,1.));
#21901=DIRECTION('',(0.61209624279065,-0.790783275974884,0.));
#21902=DIRECTION('',(0.,0.,-1.));
#21903=DIRECTION('center_axis',(0.,0.,1.));
#21904=DIRECTION('ref_axis',(-1.,0.,0.));
#21905=DIRECTION('center_axis',(0.,0.,-1.));
#21906=DIRECTION('ref_axis',(-1.,0.,0.));
#21907=DIRECTION('center_axis',(-0.900764728877053,0.434307383325507,0.));
#21908=DIRECTION('ref_axis',(0.,0.,1.));
#21909=DIRECTION('',(0.,0.,1.));
#21910=DIRECTION('',(-0.434307383325507,-0.900764728877053,0.));
#21911=DIRECTION('',(0.,0.,-1.));
#21912=DIRECTION('center_axis',(0.,0.,1.));
#21913=DIRECTION('ref_axis',(0.99756405025982,0.0697564737441876,0.));
#21914=DIRECTION('center_axis',(0.,0.,1.));
#21915=DIRECTION('ref_axis',(-0.997564050259824,-0.0697564737441253,0.));
#21916=DIRECTION('',(0.,0.,1.));
#21917=DIRECTION('center_axis',(-0.831554643148452,-0.555442954279061,0.));
#21918=DIRECTION('ref_axis',(0.,0.,1.));
#21919=DIRECTION('',(0.555442954279061,-0.831554643148452,0.));
#21920=DIRECTION('',(0.,0.,-1.));
#21921=DIRECTION('center_axis',(0.,0.,1.));
#21922=DIRECTION('ref_axis',(-1.,0.,0.));
#21923=DIRECTION('center_axis',(0.,0.,-1.));
#21924=DIRECTION('ref_axis',(-1.,0.,0.));
#21925=DIRECTION('center_axis',(-0.868274759687958,0.496083603527489,0.));
#21926=DIRECTION('ref_axis',(0.,0.,1.));
#21927=DIRECTION('',(0.,0.,1.));
#21928=DIRECTION('',(-0.496083603527489,-0.868274759687958,0.));
#21929=DIRECTION('center_axis',(0.,-9.18840917267949E-15,-1.));
#21930=DIRECTION('ref_axis',(1.,3.08644517216793E-17,0.));
#21931=DIRECTION('center_axis',(0.,0.,1.));
#21932=DIRECTION('ref_axis',(1.,6.12323399573677E-17,0.));
#21933=DIRECTION('',(0.923879532511287,3.43162438417493E-15,0.38268343236509));
#21934=DIRECTION('center_axis',(0.,0.,-1.));
#21935=DIRECTION('ref_axis',(1.,0.,0.));
#21936=DIRECTION('center_axis',(0.,0.,1.));
#21937=DIRECTION('ref_axis',(1.,0.,0.));
#21938=DIRECTION('center_axis',(0.,0.,1.));
#21939=DIRECTION('ref_axis',(1.,0.,0.));
#21940=DIRECTION('center_axis',(0.,0.,-1.));
#21941=DIRECTION('ref_axis',(1.,0.,0.));
#21942=DIRECTION('',(-0.707106781186547,-8.65956056235493E-17,-0.707106781186547));
#21943=DIRECTION('center_axis',(0.,0.,1.));
#21944=DIRECTION('ref_axis',(1.,0.,0.));
#21945=DIRECTION('center_axis',(0.,0.,1.));
#21946=DIRECTION('ref_axis',(1.,0.,0.));
#21947=DIRECTION('center_axis',(0.,0.,1.));
#21948=DIRECTION('ref_axis',(1.,0.,0.));
#21949=DIRECTION('center_axis',(0.,0.,1.));
#21950=DIRECTION('ref_axis',(1.,0.,0.));
#21951=DIRECTION('center_axis',(0.,0.,1.));
#21952=DIRECTION('ref_axis',(1.,0.,0.));
#21953=DIRECTION('center_axis',(0.,0.,1.));
#21954=DIRECTION('ref_axis',(1.,0.,0.));
#21955=DIRECTION('center_axis',(0.,0.,1.));
#21956=DIRECTION('ref_axis',(1.,0.,0.));
#21957=DIRECTION('center_axis',(0.,0.,1.));
#21958=DIRECTION('ref_axis',(1.,0.,0.));
#21959=DIRECTION('center_axis',(0.,0.,1.));
#21960=DIRECTION('ref_axis',(1.,0.,0.));
#21961=DIRECTION('center_axis',(0.,0.,1.));
#21962=DIRECTION('ref_axis',(1.,0.,0.));
#21963=DIRECTION('center_axis',(0.,0.,1.));
#21964=DIRECTION('ref_axis',(1.,0.,0.));
#21965=DIRECTION('center_axis',(0.,0.,1.));
#21966=DIRECTION('ref_axis',(1.,0.,0.));
#21967=DIRECTION('center_axis',(0.,0.,1.));
#21968=DIRECTION('ref_axis',(1.,0.,0.));
#21969=DIRECTION('center_axis',(0.,0.,1.));
#21970=DIRECTION('ref_axis',(1.,0.,0.));
#21971=DIRECTION('center_axis',(0.,0.,1.));
#21972=DIRECTION('ref_axis',(1.,0.,0.));
#21973=DIRECTION('center_axis',(0.,0.,1.));
#21974=DIRECTION('ref_axis',(1.,0.,0.));
#21975=DIRECTION('center_axis',(0.,0.,1.));
#21976=DIRECTION('ref_axis',(1.,0.,0.));
#21977=DIRECTION('center_axis',(0.,0.,1.));
#21978=DIRECTION('ref_axis',(1.,0.,0.));
#21979=DIRECTION('center_axis',(0.,0.,1.));
#21980=DIRECTION('ref_axis',(1.,0.,0.));
#21981=DIRECTION('center_axis',(0.,0.,1.));
#21982=DIRECTION('ref_axis',(1.,0.,0.));
#21983=DIRECTION('center_axis',(0.,0.,1.));
#21984=DIRECTION('ref_axis',(1.,0.,0.));
#21985=DIRECTION('center_axis',(0.,0.,1.));
#21986=DIRECTION('ref_axis',(1.,0.,0.));
#21987=DIRECTION('center_axis',(0.,0.,1.));
#21988=DIRECTION('ref_axis',(1.,0.,0.));
#21989=DIRECTION('center_axis',(0.,0.,1.));
#21990=DIRECTION('ref_axis',(1.,0.,0.));
#21991=DIRECTION('center_axis',(0.,0.,1.));
#21992=DIRECTION('ref_axis',(1.,0.,0.));
#21993=DIRECTION('center_axis',(0.,0.,1.));
#21994=DIRECTION('ref_axis',(1.,0.,0.));
#21995=DIRECTION('center_axis',(0.,0.,1.));
#21996=DIRECTION('ref_axis',(1.,0.,0.));
#21997=DIRECTION('center_axis',(0.,0.,1.));
#21998=DIRECTION('ref_axis',(1.,0.,0.));
#21999=DIRECTION('center_axis',(0.,0.,1.));
#22000=DIRECTION('ref_axis',(1.,0.,0.));
#22001=DIRECTION('center_axis',(0.,0.,1.));
#22002=DIRECTION('ref_axis',(1.,0.,0.));
#22003=DIRECTION('center_axis',(0.,0.,1.));
#22004=DIRECTION('ref_axis',(1.,0.,0.));
#22005=DIRECTION('center_axis',(0.,0.,1.));
#22006=DIRECTION('ref_axis',(1.,0.,0.));
#22007=DIRECTION('center_axis',(0.,0.,1.));
#22008=DIRECTION('ref_axis',(1.,0.,0.));
#22009=DIRECTION('center_axis',(0.,0.,1.));
#22010=DIRECTION('ref_axis',(1.,0.,0.));
#22011=DIRECTION('center_axis',(0.,0.,1.));
#22012=DIRECTION('ref_axis',(1.,0.,0.));
#22013=DIRECTION('center_axis',(0.,0.,1.));
#22014=DIRECTION('ref_axis',(1.,0.,0.));
#22015=DIRECTION('center_axis',(0.,0.,1.));
#22016=DIRECTION('ref_axis',(1.,0.,0.));
#22017=DIRECTION('center_axis',(0.,0.,1.));
#22018=DIRECTION('ref_axis',(1.,0.,0.));
#22019=DIRECTION('center_axis',(0.,0.,1.));
#22020=DIRECTION('ref_axis',(1.,0.,0.));
#22021=DIRECTION('center_axis',(0.,0.,1.));
#22022=DIRECTION('ref_axis',(1.,0.,0.));
#22023=DIRECTION('center_axis',(0.,0.,1.));
#22024=DIRECTION('ref_axis',(1.,0.,0.));
#22025=DIRECTION('center_axis',(0.,0.,1.));
#22026=DIRECTION('ref_axis',(1.,0.,0.));
#22027=DIRECTION('center_axis',(0.,0.,1.));
#22028=DIRECTION('ref_axis',(1.,0.,0.));
#22029=DIRECTION('center_axis',(0.,0.,1.));
#22030=DIRECTION('ref_axis',(1.,0.,0.));
#22031=DIRECTION('center_axis',(0.,0.,1.));
#22032=DIRECTION('ref_axis',(1.,0.,0.));
#22033=DIRECTION('center_axis',(0.,0.,1.));
#22034=DIRECTION('ref_axis',(1.,0.,0.));
#22035=DIRECTION('center_axis',(0.,0.,1.));
#22036=DIRECTION('ref_axis',(1.,0.,0.));
#22037=DIRECTION('center_axis',(0.,0.,1.));
#22038=DIRECTION('ref_axis',(1.,0.,0.));
#22039=DIRECTION('center_axis',(0.,0.,1.));
#22040=DIRECTION('ref_axis',(1.,0.,0.));
#22041=DIRECTION('center_axis',(0.,0.,1.));
#22042=DIRECTION('ref_axis',(1.,0.,0.));
#22043=DIRECTION('center_axis',(0.,0.,1.));
#22044=DIRECTION('ref_axis',(1.,0.,0.));
#22045=DIRECTION('center_axis',(0.,0.,1.));
#22046=DIRECTION('ref_axis',(1.,0.,0.));
#22047=DIRECTION('center_axis',(0.,0.,1.));
#22048=DIRECTION('ref_axis',(1.,0.,0.));
#22049=DIRECTION('center_axis',(0.,0.,1.));
#22050=DIRECTION('ref_axis',(1.,0.,0.));
#22051=DIRECTION('center_axis',(0.,0.,1.));
#22052=DIRECTION('ref_axis',(1.,0.,0.));
#22053=DIRECTION('center_axis',(0.,0.,1.));
#22054=DIRECTION('ref_axis',(1.,0.,0.));
#22055=DIRECTION('center_axis',(0.,0.,1.));
#22056=DIRECTION('ref_axis',(1.,0.,0.));
#22057=DIRECTION('center_axis',(0.,0.,1.));
#22058=DIRECTION('ref_axis',(1.,0.,0.));
#22059=DIRECTION('center_axis',(0.,0.,1.));
#22060=DIRECTION('ref_axis',(1.,0.,0.));
#22061=DIRECTION('center_axis',(0.,0.,1.));
#22062=DIRECTION('ref_axis',(1.,0.,0.));
#22063=DIRECTION('center_axis',(0.,0.,1.));
#22064=DIRECTION('ref_axis',(1.,0.,0.));
#22065=DIRECTION('center_axis',(0.,0.,1.));
#22066=DIRECTION('ref_axis',(1.,0.,0.));
#22067=DIRECTION('center_axis',(0.,0.,1.));
#22068=DIRECTION('ref_axis',(1.,0.,0.));
#22069=DIRECTION('center_axis',(0.,0.,1.));
#22070=DIRECTION('ref_axis',(1.,0.,0.));
#22071=DIRECTION('center_axis',(0.,0.,1.));
#22072=DIRECTION('ref_axis',(1.,0.,0.));
#22073=DIRECTION('center_axis',(0.,0.,1.));
#22074=DIRECTION('ref_axis',(1.,0.,0.));
#22075=DIRECTION('center_axis',(0.,0.,1.));
#22076=DIRECTION('ref_axis',(1.,0.,0.));
#22077=DIRECTION('center_axis',(0.,0.,1.));
#22078=DIRECTION('ref_axis',(1.,0.,0.));
#22079=DIRECTION('center_axis',(0.,0.,1.));
#22080=DIRECTION('ref_axis',(1.,0.,0.));
#22081=DIRECTION('center_axis',(0.,0.,1.));
#22082=DIRECTION('ref_axis',(1.,0.,0.));
#22083=DIRECTION('center_axis',(0.,0.,1.));
#22084=DIRECTION('ref_axis',(1.,0.,0.));
#22085=DIRECTION('center_axis',(0.,0.,1.));
#22086=DIRECTION('ref_axis',(1.,0.,0.));
#22087=DIRECTION('center_axis',(0.,0.,1.));
#22088=DIRECTION('ref_axis',(1.,0.,0.));
#22089=DIRECTION('center_axis',(0.,0.,1.));
#22090=DIRECTION('ref_axis',(1.,0.,0.));
#22091=DIRECTION('center_axis',(0.,0.,1.));
#22092=DIRECTION('ref_axis',(1.,0.,0.));
#22093=DIRECTION('center_axis',(0.,0.,1.));
#22094=DIRECTION('ref_axis',(1.,0.,0.));
#22095=DIRECTION('center_axis',(0.,0.,1.));
#22096=DIRECTION('ref_axis',(1.,0.,0.));
#22097=DIRECTION('center_axis',(0.,0.,1.));
#22098=DIRECTION('ref_axis',(1.,0.,0.));
#22099=DIRECTION('center_axis',(0.,0.,1.));
#22100=DIRECTION('ref_axis',(1.,0.,0.));
#22101=DIRECTION('center_axis',(0.,0.,1.));
#22102=DIRECTION('ref_axis',(1.,0.,0.));
#22103=DIRECTION('center_axis',(0.,0.,1.));
#22104=DIRECTION('ref_axis',(1.,0.,0.));
#22105=DIRECTION('center_axis',(0.,0.,1.));
#22106=DIRECTION('ref_axis',(1.,0.,0.));
#22107=DIRECTION('center_axis',(0.,0.,1.));
#22108=DIRECTION('ref_axis',(1.,0.,0.));
#22109=DIRECTION('center_axis',(0.,0.,1.));
#22110=DIRECTION('ref_axis',(1.,0.,0.));
#22111=DIRECTION('center_axis',(0.,0.,1.));
#22112=DIRECTION('ref_axis',(1.,0.,0.));
#22113=DIRECTION('center_axis',(0.,0.,1.));
#22114=DIRECTION('ref_axis',(1.,0.,0.));
#22115=DIRECTION('center_axis',(0.,0.,1.));
#22116=DIRECTION('ref_axis',(1.,0.,0.));
#22117=DIRECTION('center_axis',(0.,0.,1.));
#22118=DIRECTION('ref_axis',(1.,0.,0.));
#22119=DIRECTION('center_axis',(0.,0.,1.));
#22120=DIRECTION('ref_axis',(1.,0.,0.));
#22121=DIRECTION('center_axis',(0.,0.,1.));
#22122=DIRECTION('ref_axis',(1.,0.,0.));
#22123=DIRECTION('center_axis',(0.,0.,1.));
#22124=DIRECTION('ref_axis',(1.,0.,0.));
#22125=DIRECTION('center_axis',(0.,0.,1.));
#22126=DIRECTION('ref_axis',(1.,0.,0.));
#22127=DIRECTION('center_axis',(0.,0.,1.));
#22128=DIRECTION('ref_axis',(1.,0.,0.));
#22129=DIRECTION('center_axis',(0.,0.,1.));
#22130=DIRECTION('ref_axis',(1.,0.,0.));
#22131=DIRECTION('center_axis',(0.,0.,1.));
#22132=DIRECTION('ref_axis',(1.,0.,0.));
#22133=DIRECTION('center_axis',(0.,0.,1.));
#22134=DIRECTION('ref_axis',(1.,0.,0.));
#22135=DIRECTION('center_axis',(0.,0.,1.));
#22136=DIRECTION('ref_axis',(1.,0.,0.));
#22137=DIRECTION('center_axis',(0.,0.,1.));
#22138=DIRECTION('ref_axis',(1.,0.,0.));
#22139=DIRECTION('center_axis',(0.,0.,1.));
#22140=DIRECTION('ref_axis',(1.,0.,0.));
#22141=DIRECTION('center_axis',(0.,0.,1.));
#22142=DIRECTION('ref_axis',(1.,0.,0.));
#22143=DIRECTION('center_axis',(0.,0.,1.));
#22144=DIRECTION('ref_axis',(1.,0.,0.));
#22145=DIRECTION('center_axis',(0.,0.,1.));
#22146=DIRECTION('ref_axis',(1.,0.,0.));
#22147=DIRECTION('center_axis',(0.,0.,1.));
#22148=DIRECTION('ref_axis',(1.,0.,0.));
#22149=DIRECTION('',(0.707106781186548,8.65956056235493E-17,-0.707106781186548));
#22150=DIRECTION('center_axis',(0.,0.,-1.));
#22151=DIRECTION('ref_axis',(1.,0.,0.));
#22152=DIRECTION('center_axis',(0.,0.,1.));
#22153=DIRECTION('ref_axis',(1.,0.,0.));
#22154=DIRECTION('center_axis',(0.,0.,1.));
#22155=DIRECTION('ref_axis',(1.,0.,0.));
#22156=DIRECTION('center_axis',(0.,0.,1.));
#22157=DIRECTION('ref_axis',(1.,0.,0.));
#22158=DIRECTION('center_axis',(0.,0.,1.));
#22159=DIRECTION('ref_axis',(1.,0.,0.));
#22160=DIRECTION('center_axis',(0.,0.,-1.));
#22161=DIRECTION('ref_axis',(1.,0.,0.));
#22162=DIRECTION('center_axis',(0.,0.,1.));
#22163=DIRECTION('ref_axis',(1.,0.,0.));
#22164=DIRECTION('center_axis',(0.,0.,1.));
#22165=DIRECTION('ref_axis',(1.,0.,0.));
#22166=DIRECTION('center_axis',(0.,0.,-1.));
#22167=DIRECTION('ref_axis',(1.,0.,0.));
#22168=DIRECTION('',(0.,0.,-1.));
#22169=DIRECTION('center_axis',(0.,0.,1.));
#22170=DIRECTION('ref_axis',(1.,0.,0.));
#22171=DIRECTION('center_axis',(0.,0.,1.));
#22172=DIRECTION('ref_axis',(1.,0.,0.));
#22173=DIRECTION('',(0.707106781186548,8.65956056235493E-17,-0.707106781186548));
#22174=DIRECTION('center_axis',(0.,0.,-1.));
#22175=DIRECTION('ref_axis',(1.,0.,0.));
#22176=DIRECTION('center_axis',(0.,0.,-1.));
#22177=DIRECTION('ref_axis',(1.,0.,0.));
#22178=DIRECTION('',(0.,0.,-1.));
#22179=DIRECTION('center_axis',(0.,0.,1.));
#22180=DIRECTION('ref_axis',(1.,0.,0.));
#22181=DIRECTION('center_axis',(0.,0.,1.));
#22182=DIRECTION('ref_axis',(1.,0.,0.));
#22183=DIRECTION('',(0.707106781186548,8.65956056235493E-17,-0.707106781186548));
#22184=DIRECTION('center_axis',(0.,0.,-1.));
#22185=DIRECTION('ref_axis',(1.,0.,0.));
#22186=DIRECTION('center_axis',(0.,0.,-1.));
#22187=DIRECTION('ref_axis',(1.,0.,0.));
#22188=DIRECTION('',(0.,0.,-1.));
#22189=DIRECTION('center_axis',(0.,0.,1.));
#22190=DIRECTION('ref_axis',(1.,0.,0.));
#22191=DIRECTION('center_axis',(0.,0.,1.));
#22192=DIRECTION('ref_axis',(1.,0.,0.));
#22193=DIRECTION('',(0.707106781186548,8.65956056235493E-17,-0.707106781186548));
#22194=DIRECTION('center_axis',(0.,0.,-1.));
#22195=DIRECTION('ref_axis',(1.,0.,0.));
#22196=DIRECTION('center_axis',(0.,0.,-1.));
#22197=DIRECTION('ref_axis',(1.,0.,0.));
#22198=DIRECTION('',(0.,0.,-1.));
#22199=DIRECTION('center_axis',(0.,0.,1.));
#22200=DIRECTION('ref_axis',(1.,0.,0.));
#22201=DIRECTION('center_axis',(0.,0.,1.));
#22202=DIRECTION('ref_axis',(1.,0.,0.));
#22203=DIRECTION('',(0.707106781186548,8.65956056235493E-17,-0.707106781186548));
#22204=DIRECTION('center_axis',(0.,0.,-1.));
#22205=DIRECTION('ref_axis',(1.,0.,0.));
#22206=DIRECTION('center_axis',(0.,0.,-1.));
#22207=DIRECTION('ref_axis',(1.,0.,0.));
#22208=DIRECTION('',(0.,0.,-1.));
#22209=DIRECTION('center_axis',(0.,0.,1.));
#22210=DIRECTION('ref_axis',(1.,0.,0.));
#22211=DIRECTION('center_axis',(0.,0.,1.));
#22212=DIRECTION('ref_axis',(1.,0.,0.));
#22213=DIRECTION('',(0.707106781186545,8.6595605623549E-17,-0.70710678118655));
#22214=DIRECTION('center_axis',(0.,0.,-1.));
#22215=DIRECTION('ref_axis',(1.,0.,0.));
#22216=DIRECTION('center_axis',(0.,0.,1.));
#22217=DIRECTION('ref_axis',(1.,0.,0.));
#22218=DIRECTION('',(0.,0.,-1.));
#22219=DIRECTION('center_axis',(0.,0.,1.));
#22220=DIRECTION('ref_axis',(1.,0.,0.));
#22221=DIRECTION('center_axis',(0.,0.,1.));
#22222=DIRECTION('ref_axis',(1.,0.,0.));
#22223=DIRECTION('center_axis',(0.,0.,1.));
#22224=DIRECTION('ref_axis',(1.,0.,0.));
#22225=DIRECTION('center_axis',(0.,0.,1.));
#22226=DIRECTION('ref_axis',(1.,0.,0.));
#22227=DIRECTION('center_axis',(0.,0.,1.));
#22228=DIRECTION('ref_axis',(1.,0.,0.));
#22229=DIRECTION('center_axis',(0.,0.,1.));
#22230=DIRECTION('ref_axis',(1.,0.,0.));
#22231=DIRECTION('center_axis',(0.,0.,1.));
#22232=DIRECTION('ref_axis',(1.,0.,0.));
#22233=DIRECTION('center_axis',(0.,0.,1.));
#22234=DIRECTION('ref_axis',(1.,0.,0.));
#22235=DIRECTION('center_axis',(0.,0.,1.));
#22236=DIRECTION('ref_axis',(1.,0.,0.));
#22237=DIRECTION('center_axis',(0.,0.,1.));
#22238=DIRECTION('ref_axis',(1.,0.,0.));
#22239=DIRECTION('center_axis',(0.,0.,1.));
#22240=DIRECTION('ref_axis',(0.997564050259824,-0.0697564737441256,0.));
#22241=DIRECTION('center_axis',(0.,0.,1.));
#22242=DIRECTION('ref_axis',(0.99026806874157,-0.139173100960066,0.));
#22243=DIRECTION('center_axis',(0.,0.,1.));
#22244=DIRECTION('ref_axis',(0.978147600733805,-0.20791169081776,0.));
#22245=DIRECTION('center_axis',(0.,0.,1.));
#22246=DIRECTION('ref_axis',(0.961261695938319,-0.275637355816999,0.));
#22247=DIRECTION('center_axis',(0.,0.,1.));
#22248=DIRECTION('ref_axis',(0.939692620785909,-0.342020143325669,0.));
#22249=DIRECTION('center_axis',(0.,0.,1.));
#22250=DIRECTION('ref_axis',(0.913545457642601,-0.4067366430758,0.));
#22251=DIRECTION('center_axis',(0.,0.,1.));
#22252=DIRECTION('ref_axis',(-0.882947592858927,0.469471562785891,0.));
#22253=DIRECTION('center_axis',(0.,0.,1.));
#22254=DIRECTION('ref_axis',(0.882947592858927,-0.469471562785891,0.));
#22255=DIRECTION('center_axis',(0.,0.,1.));
#22256=DIRECTION('ref_axis',(0.882947592858927,-0.469471562785891,0.));
#22257=DIRECTION('center_axis',(0.,0.,1.));
#22258=DIRECTION('ref_axis',(0.848048096156426,-0.529919264233205,0.));
#22259=DIRECTION('center_axis',(0.,0.,1.));
#22260=DIRECTION('ref_axis',(0.809016994374947,-0.587785252292473,0.));
#22261=DIRECTION('center_axis',(0.,0.,1.));
#22262=DIRECTION('ref_axis',(0.766044443118978,-0.64278760968654,0.));
#22263=DIRECTION('center_axis',(0.,0.,1.));
#22264=DIRECTION('ref_axis',(0.719339800338651,-0.694658370458998,0.));
#22265=DIRECTION('center_axis',(0.,0.,1.));
#22266=DIRECTION('ref_axis',(0.669130606358858,-0.743144825477395,0.));
#22267=DIRECTION('center_axis',(0.,0.,1.));
#22268=DIRECTION('ref_axis',(0.615661475325659,-0.788010753606722,0.));
#22269=DIRECTION('center_axis',(0.,0.,1.));
#22270=DIRECTION('ref_axis',(0.559192903470747,-0.829037572555042,0.));
#22271=DIRECTION('center_axis',(0.,0.,1.));
#22272=DIRECTION('ref_axis',(0.5,-0.866025403784439,0.));
#22273=DIRECTION('center_axis',(0.,0.,1.));
#22274=DIRECTION('ref_axis',(0.438371146789077,-0.898794046299167,0.));
#22275=DIRECTION('center_axis',(0.,0.,1.));
#22276=DIRECTION('ref_axis',(-0.374606593415899,0.927183854566793,0.));
#22277=DIRECTION('center_axis',(0.,0.,1.));
#22278=DIRECTION('ref_axis',(0.374606593415912,-0.927183854566787,0.));
#22279=DIRECTION('center_axis',(0.,0.,1.));
#22280=DIRECTION('ref_axis',(0.374606593415912,-0.927183854566787,0.));
#22281=DIRECTION('center_axis',(0.,0.,1.));
#22282=DIRECTION('ref_axis',(0.309016994374947,-0.951056516295154,0.));
#22283=DIRECTION('center_axis',(0.,0.,1.));
#22284=DIRECTION('ref_axis',(0.241921895599667,-0.970295726275997,0.));
#22285=DIRECTION('center_axis',(0.,0.,1.));
#22286=DIRECTION('ref_axis',(0.17364817766693,-0.984807753012208,0.));
#22287=DIRECTION('center_axis',(0.,0.,1.));
#22288=DIRECTION('ref_axis',(0.104528463267653,-0.994521895368273,0.));
#22289=DIRECTION('center_axis',(0.,0.,1.));
#22290=DIRECTION('ref_axis',(0.0348994967025013,-0.999390827019096,0.));
#22291=DIRECTION('center_axis',(0.,0.,1.));
#22292=DIRECTION('ref_axis',(-0.0348994967025008,-0.999390827019096,0.));
#22293=DIRECTION('center_axis',(0.,0.,1.));
#22294=DIRECTION('ref_axis',(-0.104528463267653,-0.994521895368273,0.));
#22295=DIRECTION('center_axis',(0.,0.,1.));
#22296=DIRECTION('ref_axis',(-0.17364817766693,-0.984807753012208,0.));
#22297=DIRECTION('center_axis',(0.,0.,1.));
#22298=DIRECTION('ref_axis',(-0.241921895599668,-0.970295726275996,0.));
#22299=DIRECTION('center_axis',(0.,0.,1.));
#22300=DIRECTION('ref_axis',(0.309016994374881,0.951056516295175,0.));
#22301=DIRECTION('center_axis',(0.,0.,1.));
#22302=DIRECTION('ref_axis',(-0.309016994374948,-0.951056516295154,0.));
#22303=DIRECTION('center_axis',(0.,0.,1.));
#22304=DIRECTION('ref_axis',(-0.309016994374948,-0.951056516295153,0.));
#22305=DIRECTION('center_axis',(0.,0.,1.));
#22306=DIRECTION('ref_axis',(-0.374606593415912,-0.927183854566787,0.));
#22307=DIRECTION('center_axis',(0.,0.,1.));
#22308=DIRECTION('ref_axis',(-0.438371146789078,-0.898794046299167,0.));
#22309=DIRECTION('center_axis',(0.,0.,1.));
#22310=DIRECTION('ref_axis',(-0.5,-0.866025403784438,0.));
#22311=DIRECTION('center_axis',(0.,0.,1.));
#22312=DIRECTION('ref_axis',(-0.559192903470747,-0.829037572555042,0.));
#22313=DIRECTION('center_axis',(0.,0.,1.));
#22314=DIRECTION('ref_axis',(-0.615661475325658,-0.788010753606722,0.));
#22315=DIRECTION('center_axis',(0.,0.,1.));
#22316=DIRECTION('ref_axis',(-0.669130606358858,-0.743144825477394,0.));
#22317=DIRECTION('center_axis',(0.,0.,1.));
#22318=DIRECTION('ref_axis',(-0.719339800338651,-0.694658370458997,0.));
#22319=DIRECTION('center_axis',(0.,0.,1.));
#22320=DIRECTION('ref_axis',(-0.766044443118978,-0.642787609686539,0.));
#22321=DIRECTION('center_axis',(0.,0.,1.));
#22322=DIRECTION('ref_axis',(-0.809016994374947,-0.587785252292473,0.));
#22323=DIRECTION('center_axis',(0.,0.,1.));
#22324=DIRECTION('ref_axis',(-0.848048096156426,-0.529919264233205,0.));
#22325=DIRECTION('center_axis',(0.,0.,1.));
#22326=DIRECTION('ref_axis',(-0.882947592858927,-0.469471562785891,0.));
#22327=DIRECTION('center_axis',(0.,0.,1.));
#22328=DIRECTION('ref_axis',(-0.913545457642601,-0.4067366430758,0.));
#22329=DIRECTION('center_axis',(0.,0.,1.));
#22330=DIRECTION('ref_axis',(-0.939692620785909,-0.342020143325669,0.));
#22331=DIRECTION('center_axis',(0.,0.,1.));
#22332=DIRECTION('ref_axis',(-0.961261695938319,-0.275637355816999,0.));
#22333=DIRECTION('center_axis',(0.,0.,1.));
#22334=DIRECTION('ref_axis',(-0.978147600733805,-0.20791169081776,0.));
#22335=DIRECTION('center_axis',(0.,0.,1.));
#22336=DIRECTION('ref_axis',(-0.99026806874157,-0.139173100960066,0.));
#22337=DIRECTION('center_axis',(0.,0.,1.));
#22338=DIRECTION('ref_axis',(-0.997564050259824,-0.0697564737441253,0.));
#22339=DIRECTION('center_axis',(0.,0.,1.));
#22340=DIRECTION('ref_axis',(-1.,1.22464679914735E-16,0.));
#22341=DIRECTION('center_axis',(0.,0.,1.));
#22342=DIRECTION('ref_axis',(-0.997564050259824,0.0697564737441255,0.));
#22343=DIRECTION('center_axis',(0.,0.,1.));
#22344=DIRECTION('ref_axis',(-0.99026806874157,0.139173100960065,0.));
#22345=DIRECTION('center_axis',(0.,0.,1.));
#22346=DIRECTION('ref_axis',(-0.978147600733806,0.207911690817759,0.));
#22347=DIRECTION('center_axis',(0.,0.,1.));
#22348=DIRECTION('ref_axis',(-0.961261695938319,0.275637355816999,0.));
#22349=DIRECTION('center_axis',(0.,0.,1.));
#22350=DIRECTION('ref_axis',(-0.939692620785908,0.342020143325669,0.));
#22351=DIRECTION('center_axis',(0.,0.,1.));
#22352=DIRECTION('ref_axis',(-0.913545457642601,0.4067366430758,0.));
#22353=DIRECTION('center_axis',(0.,0.,1.));
#22354=DIRECTION('ref_axis',(-0.882947592858927,0.469471562785891,0.));
#22355=DIRECTION('center_axis',(0.,0.,1.));
#22356=DIRECTION('ref_axis',(-0.848048096156426,0.529919264233205,0.));
#22357=DIRECTION('center_axis',(0.,0.,1.));
#22358=DIRECTION('ref_axis',(-0.809016994374947,0.587785252292473,0.));
#22359=DIRECTION('center_axis',(0.,0.,1.));
#22360=DIRECTION('ref_axis',(-0.766044443118978,0.642787609686539,0.));
#22361=DIRECTION('center_axis',(0.,0.,1.));
#22362=DIRECTION('ref_axis',(-0.719339800338651,0.694658370458997,0.));
#22363=DIRECTION('center_axis',(0.,0.,1.));
#22364=DIRECTION('ref_axis',(-0.669130606358858,0.743144825477394,0.));
#22365=DIRECTION('center_axis',(0.,0.,1.));
#22366=DIRECTION('ref_axis',(-0.615661475325658,0.788010753606722,0.));
#22367=DIRECTION('center_axis',(0.,0.,1.));
#22368=DIRECTION('ref_axis',(-0.559192903470747,0.829037572555042,0.));
#22369=DIRECTION('center_axis',(0.,0.,1.));
#22370=DIRECTION('ref_axis',(-0.5,0.866025403784439,0.));
#22371=DIRECTION('center_axis',(0.,0.,1.));
#22372=DIRECTION('ref_axis',(-0.438371146789078,0.898794046299167,0.));
#22373=DIRECTION('center_axis',(0.,0.,1.));
#22374=DIRECTION('ref_axis',(-0.374606593415912,0.927183854566787,0.));
#22375=DIRECTION('center_axis',(0.,0.,1.));
#22376=DIRECTION('ref_axis',(-0.309016994374947,0.951056516295154,0.));
#22377=DIRECTION('center_axis',(0.,0.,1.));
#22378=DIRECTION('ref_axis',(-0.241921895599668,0.970295726275996,0.));
#22379=DIRECTION('center_axis',(0.,0.,1.));
#22380=DIRECTION('ref_axis',(-0.17364817766693,0.984807753012208,0.));
#22381=DIRECTION('center_axis',(0.,0.,1.));
#22382=DIRECTION('ref_axis',(-0.104528463267654,0.994521895368273,0.));
#22383=DIRECTION('center_axis',(0.,0.,1.));
#22384=DIRECTION('ref_axis',(-0.034899496702501,0.999390827019096,0.));
#22385=DIRECTION('center_axis',(0.,0.,1.));
#22386=DIRECTION('ref_axis',(-0.034899496702501,0.999390827019096,0.));
#22387=DIRECTION('center_axis',(0.,0.,1.));
#22388=DIRECTION('ref_axis',(0.0348994967025652,-0.999390827019094,0.));
#22389=DIRECTION('center_axis',(0.,0.,1.));
#22390=DIRECTION('ref_axis',(0.0348994967025011,0.999390827019096,0.));
#22391=DIRECTION('center_axis',(0.,0.,1.));
#22392=DIRECTION('ref_axis',(0.104528463267653,0.994521895368273,0.));
#22393=DIRECTION('center_axis',(0.,0.,1.));
#22394=DIRECTION('ref_axis',(0.17364817766693,0.984807753012208,0.));
#22395=DIRECTION('center_axis',(0.,0.,1.));
#22396=DIRECTION('ref_axis',(0.241921895599668,0.970295726275996,0.));
#22397=DIRECTION('center_axis',(0.,0.,1.));
#22398=DIRECTION('ref_axis',(0.309016994374948,0.951056516295154,0.));
#22399=DIRECTION('center_axis',(0.,0.,1.));
#22400=DIRECTION('ref_axis',(0.374606593415912,0.927183854566787,0.));
#22401=DIRECTION('center_axis',(0.,0.,1.));
#22402=DIRECTION('ref_axis',(0.438371146789078,0.898794046299167,0.));
#22403=DIRECTION('center_axis',(0.,0.,1.));
#22404=DIRECTION('ref_axis',(0.5,0.866025403784439,0.));
#22405=DIRECTION('center_axis',(0.,0.,1.));
#22406=DIRECTION('ref_axis',(0.559192903470747,0.829037572555042,0.));
#22407=DIRECTION('center_axis',(0.,0.,1.));
#22408=DIRECTION('ref_axis',(-0.615661475325708,-0.788010753606683,0.));
#22409=DIRECTION('center_axis',(0.,0.,1.));
#22410=DIRECTION('ref_axis',(0.615661475325658,0.788010753606722,0.));
#22411=DIRECTION('center_axis',(0.,0.,1.));
#22412=DIRECTION('ref_axis',(0.615661475325658,0.788010753606722,0.));
#22413=DIRECTION('center_axis',(0.,0.,1.));
#22414=DIRECTION('ref_axis',(0.669130606358858,0.743144825477394,0.));
#22415=DIRECTION('center_axis',(0.,0.,1.));
#22416=DIRECTION('ref_axis',(0.719339800338651,0.694658370458997,0.));
#22417=DIRECTION('center_axis',(0.,0.,1.));
#22418=DIRECTION('ref_axis',(0.766044443118978,0.642787609686539,0.));
#22419=DIRECTION('center_axis',(0.,0.,1.));
#22420=DIRECTION('ref_axis',(0.809016994374947,0.587785252292473,0.));
#22421=DIRECTION('center_axis',(0.,0.,1.));
#22422=DIRECTION('ref_axis',(0.848048096156426,0.529919264233205,0.));
#22423=DIRECTION('center_axis',(0.,0.,1.));
#22424=DIRECTION('ref_axis',(0.882947592858927,0.469471562785891,0.));
#22425=DIRECTION('center_axis',(0.,0.,1.));
#22426=DIRECTION('ref_axis',(0.913545457642601,0.4067366430758,0.));
#22427=DIRECTION('center_axis',(0.,0.,1.));
#22428=DIRECTION('ref_axis',(0.939692620785908,0.342020143325669,0.));
#22429=DIRECTION('center_axis',(0.,0.,1.));
#22430=DIRECTION('ref_axis',(0.961261695938319,0.275637355816999,0.));
#22431=DIRECTION('center_axis',(0.,0.,1.));
#22432=DIRECTION('ref_axis',(-0.978147600733819,-0.207911690817698,0.));
#22433=DIRECTION('center_axis',(0.,0.,1.));
#22434=DIRECTION('ref_axis',(0.978147600733806,0.207911690817759,0.));
#22435=DIRECTION('center_axis',(0.,0.,1.));
#22436=DIRECTION('ref_axis',(0.978147600733806,0.207911690817759,0.));
#22437=DIRECTION('center_axis',(0.,0.,1.));
#22438=DIRECTION('ref_axis',(0.99026806874157,0.139173100960065,0.));
#22439=DIRECTION('center_axis',(0.,0.,1.));
#22440=DIRECTION('ref_axis',(0.997564050259824,0.0697564737441253,0.));
#22441=DIRECTION('center_axis',(0.,0.,1.));
#22442=DIRECTION('ref_axis',(1.,0.,0.));
#22443=DIRECTION('center_axis',(0.,0.,-1.));
#22444=DIRECTION('ref_axis',(1.,0.,0.));
#22445=DIRECTION('center_axis',(0.,0.,1.));
#22446=DIRECTION('ref_axis',(1.,0.,0.));
#22447=DIRECTION('',(0.707106781186547,8.65956056235493E-17,0.707106781186548));
#22448=DIRECTION('center_axis',(0.,0.,-1.));
#22449=DIRECTION('ref_axis',(1.,0.,0.));
#22450=DIRECTION('center_axis',(0.,0.,1.));
#22451=DIRECTION('ref_axis',(1.,0.,0.));
#22452=DIRECTION('',(0.707106781186547,8.65956056235493E-17,0.707106781186548));
#22453=DIRECTION('center_axis',(0.,0.,-1.));
#22454=DIRECTION('ref_axis',(1.,0.,0.));
#22455=DIRECTION('center_axis',(0.,0.,1.));
#22456=DIRECTION('ref_axis',(1.,0.,0.));
#22457=DIRECTION('',(0.707106781186547,8.65956056235493E-17,0.707106781186548));
#22458=DIRECTION('center_axis',(0.,0.,-1.));
#22459=DIRECTION('ref_axis',(1.,0.,0.));
#22460=DIRECTION('center_axis',(0.,0.,1.));
#22461=DIRECTION('ref_axis',(1.,0.,0.));
#22462=DIRECTION('',(0.707106781186547,8.65956056235493E-17,0.707106781186548));
#22463=DIRECTION('center_axis',(0.,0.,-1.));
#22464=DIRECTION('ref_axis',(1.,0.,0.));
#22465=DIRECTION('center_axis',(0.,0.,1.));
#22466=DIRECTION('ref_axis',(1.,0.,0.));
#22467=DIRECTION('',(0.707106781186547,8.65956056235493E-17,0.707106781186548));
#22468=DIRECTION('center_axis',(0.,0.,-1.));
#22469=DIRECTION('ref_axis',(1.,0.,0.));
#22470=DIRECTION('',(0.,0.,-1.));
#22471=DIRECTION('center_axis',(0.,0.,1.));
#22472=DIRECTION('ref_axis',(1.,0.,0.));
#22473=DIRECTION('center_axis',(0.,0.,1.));
#22474=DIRECTION('ref_axis',(1.,0.,0.));
#22475=DIRECTION('axis',(0.,0.,1.));
#22476=DIRECTION('refdir',(1.,0.,0.));
#22477=DIRECTION('center_axis',(1.,0.,0.));
#22478=DIRECTION('ref_axis',(0.,0.935047775444299,0.354521730838417));
#22479=DIRECTION('',(-1.,0.,0.));
#22480=DIRECTION('center_axis',(-1.,0.,0.));
#22481=DIRECTION('ref_axis',(0.,1.,0.));
#22482=DIRECTION('center_axis',(1.,0.,0.));
#22483=DIRECTION('ref_axis',(0.,1.,0.));
#22484=DIRECTION('',(-1.,0.,0.));
#22485=DIRECTION('center_axis',(1.,0.,0.));
#22486=DIRECTION('ref_axis',(0.,1.,0.));
#22487=DIRECTION('',(-1.,0.,0.));
#22488=DIRECTION('center_axis',(1.,0.,0.));
#22489=DIRECTION('ref_axis',(0.,1.,0.));
#22490=DIRECTION('',(-1.,0.,0.));
#22491=DIRECTION('center_axis',(1.,0.,0.));
#22492=DIRECTION('ref_axis',(0.,1.,0.));
#22493=DIRECTION('',(-1.,0.,0.));
#22494=DIRECTION('center_axis',(1.,0.,0.));
#22495=DIRECTION('ref_axis',(0.,1.,0.));
#22496=DIRECTION('',(-1.,0.,0.));
#22497=DIRECTION('center_axis',(1.,0.,0.));
#22498=DIRECTION('ref_axis',(0.,1.,0.));
#22499=DIRECTION('',(-1.,0.,0.));
#22500=DIRECTION('center_axis',(1.,0.,0.));
#22501=DIRECTION('ref_axis',(0.,1.,0.));
#22502=DIRECTION('',(-1.,0.,0.));
#22503=DIRECTION('center_axis',(1.,0.,0.));
#22504=DIRECTION('ref_axis',(0.,1.,0.));
#22505=DIRECTION('',(-1.,0.,0.));
#22506=DIRECTION('center_axis',(1.,0.,0.));
#22507=DIRECTION('ref_axis',(0.,1.,0.));
#22508=DIRECTION('',(-1.,0.,0.));
#22509=DIRECTION('center_axis',(1.,0.,0.));
#22510=DIRECTION('ref_axis',(0.,1.,0.));
#22511=DIRECTION('',(-1.,0.,0.));
#22512=DIRECTION('center_axis',(1.,0.,0.));
#22513=DIRECTION('ref_axis',(0.,-0.354512791606023,-0.935051164689775));
#22514=DIRECTION('',(-1.,0.,0.));
#22515=DIRECTION('center_axis',(1.,0.,0.));
#22516=DIRECTION('ref_axis',(0.,1.,0.));
#22517=DIRECTION('center_axis',(1.,0.,0.));
#22518=DIRECTION('ref_axis',(0.,0.793330745045896,-0.608790874574286));
#22519=DIRECTION('',(1.,1.22464679914735E-16,5.71605565684554E-30));
#22520=DIRECTION('center_axis',(-1.,0.,0.));
#22521=DIRECTION('ref_axis',(0.,1.,4.65526718641507E-14));
#22522=DIRECTION('center_axis',(1.,0.,0.));
#22523=DIRECTION('ref_axis',(0.,1.,4.65526718641507E-14));
#22524=DIRECTION('',(1.,1.22464679914735E-16,5.71605565684554E-30));
#22525=DIRECTION('center_axis',(1.,0.,0.));
#22526=DIRECTION('ref_axis',(0.,1.,4.65526718641507E-14));
#22527=DIRECTION('',(1.,1.22464679914735E-16,5.71605565684554E-30));
#22528=DIRECTION('center_axis',(1.,0.,0.));
#22529=DIRECTION('ref_axis',(0.,1.,4.65526718641507E-14));
#22530=DIRECTION('',(1.,1.22464679914735E-16,5.71605565684554E-30));
#22531=DIRECTION('center_axis',(1.,0.,0.));
#22532=DIRECTION('ref_axis',(0.,1.,4.65526718641507E-14));
#22533=DIRECTION('',(1.,1.22464679914735E-16,5.71605565684554E-30));
#22534=DIRECTION('center_axis',(1.,0.,0.));
#22535=DIRECTION('ref_axis',(0.,1.,4.65526718641507E-14));
#22536=DIRECTION('',(1.,1.22464679914735E-16,5.71605565684554E-30));
#22537=DIRECTION('center_axis',(1.,0.,0.));
#22538=DIRECTION('ref_axis',(0.,1.,4.65526718641507E-14));
#22539=DIRECTION('',(1.,1.22464679914735E-16,5.71605565684554E-30));
#22540=DIRECTION('center_axis',(1.,0.,0.));
#22541=DIRECTION('ref_axis',(0.,1.,4.65526718641507E-14));
#22542=DIRECTION('',(1.,1.22464679914735E-16,5.71605565684554E-30));
#22543=DIRECTION('center_axis',(1.,0.,0.));
#22544=DIRECTION('ref_axis',(0.,1.,4.65526718641507E-14));
#22545=DIRECTION('',(1.,1.22464679914735E-16,5.71605565684554E-30));
#22546=DIRECTION('center_axis',(1.,0.,0.));
#22547=DIRECTION('ref_axis',(0.,1.,4.65526718641507E-14));
#22548=DIRECTION('',(1.,1.22464679914735E-16,5.71605565684554E-30));
#22549=DIRECTION('center_axis',(1.,0.,0.));
#22550=DIRECTION('ref_axis',(0.,1.,4.65526718641507E-14));
#22551=DIRECTION('',(1.,1.22464679914735E-16,5.71605565684554E-30));
#22552=DIRECTION('center_axis',(1.,0.,0.));
#22553=DIRECTION('ref_axis',(0.,-0.60879845580878,0.793324927255437));
#22554=DIRECTION('',(1.,1.22464679914735E-16,5.71605565684554E-30));
#22555=DIRECTION('center_axis',(1.,0.,0.));
#22556=DIRECTION('ref_axis',(0.,1.,4.65526718641507E-14));
#22557=DIRECTION('center_axis',(1.,0.,0.));
#22558=DIRECTION('ref_axis',(0.,1.,4.65526718641507E-14));
#22559=DIRECTION('center_axis',(-1.,0.,0.));
#22560=DIRECTION('ref_axis',(0.,0.,1.));
#22561=DIRECTION('center_axis',(1.,0.,0.));
#22562=DIRECTION('ref_axis',(0.,0.,-1.));
#22563=DIRECTION('center_axis',(1.,0.,0.));
#22564=DIRECTION('ref_axis',(0.,1.,0.));
#22565=DIRECTION('center_axis',(1.,0.,0.));
#22566=DIRECTION('ref_axis',(0.,1.,0.));
#22567=DIRECTION('center_axis',(1.,0.,0.));
#22568=DIRECTION('ref_axis',(0.,0.,-1.));
#22569=DIRECTION('',(-1.,0.,0.));
#22570=DIRECTION('center_axis',(-1.,0.,0.));
#22571=DIRECTION('ref_axis',(0.,0.,1.));
#22572=DIRECTION('center_axis',(1.,0.,0.));
#22573=DIRECTION('ref_axis',(0.,0.,-1.));
#22574=DIRECTION('center_axis',(1.,0.,0.));
#22575=DIRECTION('ref_axis',(0.,1.,0.));
#22576=DIRECTION('center_axis',(1.,0.,0.));
#22577=DIRECTION('ref_axis',(0.,0.,-1.));
#22578=DIRECTION('',(-1.,0.,0.));
#22579=DIRECTION('center_axis',(-1.,0.,0.));
#22580=DIRECTION('ref_axis',(0.,1.,0.));
#22581=DIRECTION('center_axis',(1.,0.,0.));
#22582=DIRECTION('ref_axis',(0.,0.,-1.));
#22583=DIRECTION('',(-0.707106781186547,-0.707106781186548,-8.65956056235493E-17));
#22584=DIRECTION('center_axis',(1.,0.,0.));
#22585=DIRECTION('ref_axis',(0.,0.,-1.));
#22586=DIRECTION('axis',(0.,0.,1.));
#22587=DIRECTION('refdir',(1.,0.,0.));
#22588=DIRECTION('center_axis',(1.,0.,0.));
#22589=DIRECTION('ref_axis',(0.,1.,0.));
#22590=DIRECTION('',(-1.,0.,0.));
#22591=DIRECTION('center_axis',(-1.,0.,0.));
#22592=DIRECTION('ref_axis',(0.,1.,0.));
#22593=DIRECTION('center_axis',(1.,0.,0.));
#22594=DIRECTION('ref_axis',(0.,1.,0.));
#22595=DIRECTION('',(-1.,0.,0.));
#22596=DIRECTION('center_axis',(1.,0.,0.));
#22597=DIRECTION('ref_axis',(0.,1.,0.));
#22598=DIRECTION('',(-1.,0.,0.));
#22599=DIRECTION('center_axis',(1.,0.,0.));
#22600=DIRECTION('ref_axis',(0.,1.,0.));
#22601=DIRECTION('',(-1.,0.,0.));
#22602=DIRECTION('center_axis',(1.,0.,0.));
#22603=DIRECTION('ref_axis',(0.,1.,0.));
#22604=DIRECTION('',(-1.,0.,0.));
#22605=DIRECTION('center_axis',(1.,0.,0.));
#22606=DIRECTION('ref_axis',(0.,1.,0.));
#22607=DIRECTION('',(-1.,0.,0.));
#22608=DIRECTION('center_axis',(1.,0.,0.));
#22609=DIRECTION('ref_axis',(0.,-0.289393351880426,-0.957210263154032));
#22610=DIRECTION('',(1.,0.,0.));
#22611=DIRECTION('center_axis',(1.,0.,0.));
#22612=DIRECTION('ref_axis',(0.,1.,9.11763443140316E-15));
#22613=DIRECTION('center_axis',(1.,0.,0.));
#22614=DIRECTION('ref_axis',(0.,1.,9.11763443140316E-15));
#22615=DIRECTION('',(1.,0.,0.));
#22616=DIRECTION('center_axis',(1.,0.,0.));
#22617=DIRECTION('ref_axis',(0.,1.,9.11763443140316E-15));
#22618=DIRECTION('',(1.,0.,0.));
#22619=DIRECTION('center_axis',(1.,0.,0.));
#22620=DIRECTION('ref_axis',(0.,1.,9.11763443140316E-15));
#22621=DIRECTION('',(1.,0.,0.));
#22622=DIRECTION('center_axis',(1.,0.,0.));
#22623=DIRECTION('ref_axis',(0.,1.,9.11763443140316E-15));
#22624=DIRECTION('',(1.,0.,0.));
#22625=DIRECTION('center_axis',(1.,0.,0.));
#22626=DIRECTION('ref_axis',(0.,1.,9.11763443140316E-15));
#22627=DIRECTION('',(1.,0.,0.));
#22628=DIRECTION('center_axis',(1.,0.,0.));
#22629=DIRECTION('ref_axis',(0.,0.,-1.));
#22630=DIRECTION('center_axis',(-1.,0.,0.));
#22631=DIRECTION('ref_axis',(0.,1.,0.));
#22632=DIRECTION('center_axis',(-1.,0.,0.));
#22633=DIRECTION('ref_axis',(0.,1.,0.));
#22634=DIRECTION('center_axis',(1.,0.,0.));
#22635=DIRECTION('ref_axis',(0.,0.889041585325826,0.457826451356126));
#22636=DIRECTION('center_axis',(-1.,0.,0.));
#22637=DIRECTION('ref_axis',(0.,1.,9.11763443140316E-15));
#22638=DIRECTION('center_axis',(1.,0.,0.));
#22639=DIRECTION('ref_axis',(0.,0.929925526089149,-0.367747897244593));
#22640=DIRECTION('center_axis',(-1.,0.,0.));
#22641=DIRECTION('ref_axis',(0.,1.,0.));
#22642=DIRECTION('center_axis',(-1.,0.,0.));
#22643=DIRECTION('ref_axis',(0.,0.,1.));
#22644=DIRECTION('center_axis',(1.,0.,0.));
#22645=DIRECTION('ref_axis',(0.,0.,-1.));
#22646=DIRECTION('center_axis',(1.,0.,0.));
#22647=DIRECTION('ref_axis',(0.,1.,0.));
#22648=DIRECTION('center_axis',(1.,0.,0.));
#22649=DIRECTION('ref_axis',(0.,0.,-1.));
#22650=DIRECTION('',(-0.707106781186547,0.707106781186548,8.65956056235494E-17));
#22651=DIRECTION('center_axis',(1.,0.,0.));
#22652=DIRECTION('ref_axis',(0.,1.,0.));
#22653=DIRECTION('center_axis',(1.,0.,0.));
#22654=DIRECTION('ref_axis',(0.,0.,-1.));
#22655=DIRECTION('',(-1.,0.,0.));
#22656=DIRECTION('center_axis',(1.,0.,0.));
#22657=DIRECTION('ref_axis',(0.,0.,-1.));
#22658=DIRECTION('center_axis',(-1.,0.,0.));
#22659=DIRECTION('ref_axis',(0.,1.,0.));
#22660=DIRECTION('center_axis',(1.,0.,0.));
#22661=DIRECTION('ref_axis',(0.,0.,-1.));
#22662=DIRECTION('',(-0.707106781186544,-0.707106781186551,-8.65956056235498E-17));
#22663=DIRECTION('center_axis',(1.,0.,0.));
#22664=DIRECTION('ref_axis',(0.,0.,-1.));
#22665=DIRECTION('axis',(0.,0.,1.));
#22666=DIRECTION('refdir',(1.,0.,0.));
#22667=DIRECTION('center_axis',(-1.,0.,-1.6002526653361E-16));
#22668=DIRECTION('ref_axis',(0.,-1.,-6.12323399573677E-17));
#22669=DIRECTION('center_axis',(-1.,0.,0.));
#22670=DIRECTION('ref_axis',(0.,-1.,-6.12323399573677E-17));
#22671=DIRECTION('center_axis',(-1.,0.,0.));
#22672=DIRECTION('ref_axis',(0.,-1.,-6.12323399573677E-17));
#22673=DIRECTION('',(-0.35737274613036,0.933961840935295,1.14377337902718E-16));
#22674=DIRECTION('center_axis',(1.,0.,0.));
#22675=DIRECTION('ref_axis',(0.,-1.,-6.12323399573676E-17));
#22676=DIRECTION('center_axis',(1.,0.,0.));
#22677=DIRECTION('ref_axis',(0.,-1.,-6.12323399573676E-17));
#22678=DIRECTION('center_axis',(-1.,0.,0.));
#22679=DIRECTION('ref_axis',(0.,1.,0.));
#22680=DIRECTION('',(-0.581238193719096,-0.813733471206735,-9.96536090872393E-17));
#22681=DIRECTION('center_axis',(1.,0.,0.));
#22682=DIRECTION('ref_axis',(0.,0.,-1.));
#22683=DIRECTION('center_axis',(-1.,0.,0.));
#22684=DIRECTION('ref_axis',(0.,1.,0.));
#22685=DIRECTION('center_axis',(1.,0.,0.));
#22686=DIRECTION('ref_axis',(0.,0.,-1.));
#22687=DIRECTION('',(-0.110431526074847,-0.993883734673619,-1.21715653439266E-16));
#22688=DIRECTION('center_axis',(-1.,0.,0.));
#22689=DIRECTION('ref_axis',(0.,0.,1.));
#22690=DIRECTION('center_axis',(1.,0.,0.));
#22691=DIRECTION('ref_axis',(0.,0.,-1.));
#22692=DIRECTION('center_axis',(1.,0.,0.));
#22693=DIRECTION('ref_axis',(0.,0.,-1.));
#22694=DIRECTION('center_axis',(1.,0.,0.));
#22695=DIRECTION('ref_axis',(0.,1.,0.));
#22696=DIRECTION('',(1.,0.,0.));
#22697=DIRECTION('center_axis',(-1.,0.,0.));
#22698=DIRECTION('ref_axis',(0.,1.,0.));
#22699=DIRECTION('center_axis',(1.,0.,0.));
#22700=DIRECTION('ref_axis',(0.,1.,0.));
#22701=DIRECTION('',(1.,0.,0.));
#22702=DIRECTION('center_axis',(1.,0.,0.));
#22703=DIRECTION('ref_axis',(0.,1.,0.));
#22704=DIRECTION('center_axis',(1.,0.,0.));
#22705=DIRECTION('ref_axis',(0.,0.,-1.));
#22706=DIRECTION('center_axis',(1.,0.,0.));
#22707=DIRECTION('ref_axis',(0.,1.,0.));
#22708=DIRECTION('center_axis',(1.,0.,0.));
#22709=DIRECTION('ref_axis',(0.,0.,-1.));
#22710=DIRECTION('',(-1.,0.,0.));
#22711=DIRECTION('center_axis',(1.,0.,0.));
#22712=DIRECTION('ref_axis',(0.,0.,-1.));
#22713=DIRECTION('center_axis',(-1.,0.,0.));
#22714=DIRECTION('ref_axis',(0.,0.,1.));
#22715=DIRECTION('center_axis',(1.,0.,0.));
#22716=DIRECTION('ref_axis',(0.,0.,-1.));
#22717=DIRECTION('center_axis',(1.,0.,0.));
#22718=DIRECTION('ref_axis',(0.,1.,0.));
#22719=DIRECTION('',(-1.,0.,0.));
#22720=DIRECTION('center_axis',(1.,0.,0.));
#22721=DIRECTION('ref_axis',(0.,0.,-1.));
#22722=DIRECTION('center_axis',(-1.,0.,0.));
#22723=DIRECTION('ref_axis',(0.,0.,1.));
#22724=DIRECTION('axis',(0.,0.,1.));
#22725=DIRECTION('refdir',(1.,0.,0.));
#22726=DIRECTION('center_axis',(1.,0.,0.));
#22727=DIRECTION('ref_axis',(0.,1.,0.));
#22728=DIRECTION('center_axis',(1.,0.,0.));
#22729=DIRECTION('ref_axis',(0.,0.,-1.));
#22730=DIRECTION('',(-1.,0.,0.));
#22731=DIRECTION('center_axis',(1.,0.,0.));
#22732=DIRECTION('ref_axis',(0.,0.,-1.));
#22733=DIRECTION('center_axis',(-1.,0.,0.));
#22734=DIRECTION('ref_axis',(0.,0.,1.));
#22735=DIRECTION('center_axis',(1.,0.,0.));
#22736=DIRECTION('ref_axis',(0.,0.,-1.));
#22737=DIRECTION('center_axis',(1.,0.,0.));
#22738=DIRECTION('ref_axis',(0.,1.,0.));
#22739=DIRECTION('center_axis',(1.,0.,0.));
#22740=DIRECTION('ref_axis',(0.,0.,-1.));
#22741=DIRECTION('',(-1.,0.,0.));
#22742=DIRECTION('center_axis',(1.,0.,0.));
#22743=DIRECTION('ref_axis',(0.,0.,-1.));
#22744=DIRECTION('axis',(0.,0.,1.));
#22745=DIRECTION('refdir',(1.,0.,0.));
#22746=DIRECTION('center_axis',(-1.,0.,0.));
#22747=DIRECTION('ref_axis',(0.,-1.,0.));
#22748=DIRECTION('center_axis',(-1.,0.,0.));
#22749=DIRECTION('ref_axis',(0.,-1.,0.));
#22750=DIRECTION('',(-0.707106781186547,0.707106781186548,8.65956056235494E-17));
#22751=DIRECTION('center_axis',(1.,0.,0.));
#22752=DIRECTION('ref_axis',(0.,-1.,0.));
#22753=DIRECTION('center_axis',(1.,0.,0.));
#22754=DIRECTION('ref_axis',(0.,-1.,0.));
#22755=DIRECTION('center_axis',(1.,0.,0.));
#22756=DIRECTION('ref_axis',(0.,1.,0.));
#22757=DIRECTION('',(-1.,0.,0.));
#22758=DIRECTION('center_axis',(1.,0.,0.));
#22759=DIRECTION('ref_axis',(0.,0.,-1.));
#22760=DIRECTION('center_axis',(1.,0.,0.));
#22761=DIRECTION('ref_axis',(0.,0.,-1.));
#22762=DIRECTION('center_axis',(1.,0.,0.));
#22763=DIRECTION('ref_axis',(0.,0.,-1.));
#22764=DIRECTION('center_axis',(1.,0.,0.));
#22765=DIRECTION('ref_axis',(0.,1.,0.));
#22766=DIRECTION('',(-1.,0.,0.));
#22767=DIRECTION('center_axis',(1.,0.,0.));
#22768=DIRECTION('ref_axis',(0.,0.,-1.));
#22769=DIRECTION('center_axis',(-1.,0.,0.));
#22770=DIRECTION('ref_axis',(0.,0.,1.));
#22771=DIRECTION('center_axis',(1.,0.,0.));
#22772=DIRECTION('ref_axis',(0.,0.,-1.));
#22773=DIRECTION('center_axis',(1.,0.,0.));
#22774=DIRECTION('ref_axis',(0.,1.,0.));
#22775=DIRECTION('',(-0.707106781186547,0.707106781186548,8.65956056235494E-17));
#22776=DIRECTION('axis',(0.,0.,1.));
#22777=DIRECTION('refdir',(1.,0.,0.));
#22778=DIRECTION('center_axis',(-1.,0.,0.));
#22779=DIRECTION('ref_axis',(0.,0.,-1.));
#22780=DIRECTION('center_axis',(-1.,0.,0.));
#22781=DIRECTION('ref_axis',(0.,0.,-1.));
#22782=DIRECTION('',(0.707106781186547,-8.65956056235494E-17,-0.707106781186548));
#22783=DIRECTION('center_axis',(1.,0.,0.));
#22784=DIRECTION('ref_axis',(0.,0.,-1.));
#22785=DIRECTION('center_axis',(1.,0.,0.));
#22786=DIRECTION('ref_axis',(0.,0.,-1.));
#22787=DIRECTION('',(1.,0.,0.));
#22788=DIRECTION('center_axis',(-1.,0.,0.));
#22789=DIRECTION('ref_axis',(0.,0.,-1.));
#22790=DIRECTION('center_axis',(1.,0.,0.));
#22791=DIRECTION('ref_axis',(0.,0.,-1.));
#22792=DIRECTION('center_axis',(-1.,0.,0.));
#22793=DIRECTION('ref_axis',(0.,1.,0.));
#22794=DIRECTION('center_axis',(1.,0.,0.));
#22795=DIRECTION('ref_axis',(0.,0.,-1.));
#22796=DIRECTION('center_axis',(1.,0.,0.));
#22797=DIRECTION('ref_axis',(0.,0.,-1.));
#22798=DIRECTION('',(-0.707106781186547,8.65956056235493E-17,-0.707106781186547));
#22799=DIRECTION('center_axis',(1.,0.,0.));
#22800=DIRECTION('ref_axis',(0.,0.,-1.));
#22801=DIRECTION('center_axis',(-1.,0.,0.));
#22802=DIRECTION('ref_axis',(0.,1.,0.));
#22803=DIRECTION('center_axis',(-1.,0.,-2.85780237930534E-15));
#22804=DIRECTION('ref_axis',(0.,1.,3.18764105070188E-17));
#22805=DIRECTION('',(-0.261545900451064,-0.965191039099122,-8.96415134046473E-16));
#22806=DIRECTION('center_axis',(1.,0.,0.));
#22807=DIRECTION('ref_axis',(0.,1.,6.12323399573677E-17));
#22808=DIRECTION('center_axis',(1.,0.,0.));
#22809=DIRECTION('ref_axis',(0.,1.,6.12323399573677E-17));
#22810=DIRECTION('center_axis',(1.,0.,0.));
#22811=DIRECTION('ref_axis',(0.,1.,6.12323399573677E-17));
#22812=DIRECTION('center_axis',(1.,0.,0.));
#22813=DIRECTION('ref_axis',(0.,1.,6.12323399573677E-17));
#22814=DIRECTION('center_axis',(1.,0.,0.));
#22815=DIRECTION('ref_axis',(0.,1.,6.12323399573677E-17));
#22816=DIRECTION('center_axis',(1.,0.,0.));
#22817=DIRECTION('ref_axis',(0.,1.,6.12323399573677E-17));
#22818=DIRECTION('center_axis',(-1.,0.,0.));
#22819=DIRECTION('ref_axis',(0.,1.,0.));
#22820=DIRECTION('center_axis',(-1.,0.,0.));
#22821=DIRECTION('ref_axis',(0.,1.,0.));
#22822=DIRECTION('center_axis',(-1.,0.,0.));
#22823=DIRECTION('ref_axis',(0.,1.,0.));
#22824=DIRECTION('center_axis',(-1.,0.,0.));
#22825=DIRECTION('ref_axis',(0.,1.,0.));
#22826=DIRECTION('center_axis',(-1.,0.,0.));
#22827=DIRECTION('ref_axis',(0.,1.,0.));
#22828=DIRECTION('center_axis',(-1.,0.,0.));
#22829=DIRECTION('ref_axis',(0.,1.,0.));
#22830=DIRECTION('center_axis',(0.367220154484801,0.805519719562706,-0.46506702692814));
#22831=DIRECTION('ref_axis',(-0.784831896934838,0.,-0.61970871669976));
#22832=DIRECTION('',(0.,-0.499999999999997,-0.86602540378444));
#22833=DIRECTION('center_axis',(0.3672201544848,-9.20177782101458E-13,-0.93013405385469));
#22834=DIRECTION('ref_axis',(-0.93013405385469,0.,-0.3672201544848));
#22835=DIRECTION('',(-3.05232172441836E-15,-1.,0.));
#22836=DIRECTION('center_axis',(0.367220154484803,0.805519719563624,0.465067026926548));
#22837=DIRECTION('ref_axis',(0.784831896933805,0.,-0.619708716701069));
#22838=DIRECTION('',(0.,0.499999999999999,-0.866025403784439));
#22839=DIRECTION('center_axis',(0.367220154484804,-0.805519719563622,-0.46506702692655));
#22840=DIRECTION('ref_axis',(-0.784831896933805,0.,-0.619708716701069));
#22841=DIRECTION('',(9.15696517325506E-15,-0.499999999999999,0.866025403784439));
#22842=DIRECTION('center_axis',(0.3672201544848,9.17903343076173E-13,0.93013405385469));
#22843=DIRECTION('ref_axis',(0.93013405385469,0.,-0.3672201544848));
#22844=DIRECTION('',(-1.52616086220918E-15,1.,3.05232172441836E-15));
#22845=DIRECTION('center_axis',(0.367220154484798,-0.805519719562705,0.465067026928142));
#22846=DIRECTION('ref_axis',(0.784831896934842,0.,-0.619708716699756));
#22847=DIRECTION('',(-3.05232172441835E-15,0.499999999999999,0.866025403784439));
#22848=DIRECTION('center_axis',(0.,-0.866025403784439,0.499999999999999));
#22849=DIRECTION('ref_axis',(0.,-0.499999999999999,-0.866025403784439));
#22850=DIRECTION('',(1.,0.,0.));
#22851=DIRECTION('',(-1.,0.,0.));
#22852=DIRECTION('center_axis',(0.,-3.05232172441836E-15,1.));
#22853=DIRECTION('ref_axis',(1.,0.,0.));
#22854=DIRECTION('',(1.,0.,0.));
#22855=DIRECTION('',(-1.,0.,0.));
#22856=DIRECTION('center_axis',(0.,-0.866025403784439,-0.499999999999999));
#22857=DIRECTION('ref_axis',(0.,0.499999999999999,-0.866025403784439));
#22858=DIRECTION('',(1.,0.,0.));
#22859=DIRECTION('',(-1.,0.,0.));
#22860=DIRECTION('center_axis',(0.,0.866025403784439,0.499999999999999));
#22861=DIRECTION('ref_axis',(0.,-0.499999999999999,0.866025403784439));
#22862=DIRECTION('',(1.,0.,0.));
#22863=DIRECTION('',(-1.,0.,0.));
#22864=DIRECTION('center_axis',(0.,0.,-1.));
#22865=DIRECTION('ref_axis',(-1.,0.,0.));
#22866=DIRECTION('',(1.,0.,0.));
#22867=DIRECTION('',(-1.,0.,0.));
#22868=DIRECTION('center_axis',(0.,0.86602540378444,-0.499999999999997));
#22869=DIRECTION('ref_axis',(0.,0.499999999999997,0.86602540378444));
#22870=DIRECTION('',(1.,0.,0.));
#22871=DIRECTION('',(-1.,0.,0.));
#22872=DIRECTION('center_axis',(0.,0.5,0.866025403784439));
#22873=DIRECTION('ref_axis',(0.,-0.866025403784439,0.5));
#22874=DIRECTION('center_axis',(0.,1.,-3.84592537276713E-16));
#22875=DIRECTION('ref_axis',(0.,3.84592537276713E-16,1.));
#22876=DIRECTION('center_axis',(0.,0.5,-0.866025403784439));
#22877=DIRECTION('ref_axis',(0.,0.866025403784439,0.5));
#22878=DIRECTION('center_axis',(1.,0.,0.));
#22879=DIRECTION('ref_axis',(0.,1.,0.));
#22880=DIRECTION('',(0.504883518856957,-0.863187483914483,-1.05709978923993E-16));
#22881=DIRECTION('center_axis',(0.,-0.5,-0.866025403784439));
#22882=DIRECTION('ref_axis',(0.,0.866025403784439,-0.5));
#22883=DIRECTION('center_axis',(0.,-1.,-1.92296268638356E-16));
#22884=DIRECTION('ref_axis',(0.,1.92296268638356E-16,-1.));
#22885=DIRECTION('center_axis',(0.,-0.5,0.866025403784439));
#22886=DIRECTION('ref_axis',(0.,-0.866025403784439,-0.5));
#22887=DIRECTION('axis',(0.,0.,1.));
#22888=DIRECTION('refdir',(1.,0.,0.));
#22889=DIRECTION('center_axis',(6.12323399573677E-17,0.,1.));
#22890=DIRECTION('ref_axis',(1.,0.,0.));
#22891=DIRECTION('center_axis',(1.22464679914735E-16,-1.,0.));
#22892=DIRECTION('ref_axis',(-1.,-1.22464679914735E-16,0.));
#22893=DIRECTION('axis',(0.,0.,1.));
#22894=DIRECTION('refdir',(1.,0.,0.));
#22895=DIRECTION('center_axis',(0.10451361405356,-0.00184126643092401,0.994521751504407));
#22896=DIRECTION('ref_axis',(-0.994367449791123,0.0175182479515601,0.104529832031847));
#22897=DIRECTION('center_axis',(0.104513613956506,0.00184126640140064,0.994521751514661));
#22898=DIRECTION('ref_axis',(0.631399161915391,-0.77273549595271,-0.0649226588123218));
#22899=DIRECTION('center_axis',(0.104513613956506,0.00184126640140064,0.994521751514661));
#22900=DIRECTION('ref_axis',(0.631399161915391,-0.77273549595271,-0.0649226588123217));
#22901=DIRECTION('center_axis',(0.10451361405356,-0.00184126643092401,0.994521751504407));
#22902=DIRECTION('ref_axis',(-0.994367449791123,0.0175182479515601,0.104529832031847));
#22903=DIRECTION('axis',(0.,0.,1.));
#22904=DIRECTION('refdir',(1.,0.,0.));
#22905=DIRECTION('center_axis',(1.,0.,0.));
#22906=DIRECTION('ref_axis',(0.,1.,0.));
#22907=DIRECTION('',(-1.,0.,0.));
#22908=DIRECTION('center_axis',(1.,0.,0.));
#22909=DIRECTION('ref_axis',(0.,1.,0.));
#22910=DIRECTION('center_axis',(1.,0.,0.));
#22911=DIRECTION('ref_axis',(0.,1.,0.));
#22912=DIRECTION('',(-1.,0.,0.));
#22913=DIRECTION('center_axis',(1.,0.,0.));
#22914=DIRECTION('ref_axis',(0.,1.,0.));
#22915=DIRECTION('',(-1.,0.,0.));
#22916=DIRECTION('center_axis',(1.,0.,0.));
#22917=DIRECTION('ref_axis',(0.,1.,0.));
#22918=DIRECTION('',(-1.,0.,0.));
#22919=DIRECTION('center_axis',(1.,0.,0.));
#22920=DIRECTION('ref_axis',(6.95715643956108E-17,-0.0863639019455519,-0.996263658094954));
#22921=DIRECTION('',(1.,0.,0.));
#22922=DIRECTION('center_axis',(1.,0.,0.));
#22923=DIRECTION('ref_axis',(6.95715643956108E-17,1.,6.84751808553105E-15));
#22924=DIRECTION('center_axis',(1.,0.,0.));
#22925=DIRECTION('ref_axis',(6.95715643956108E-17,1.,6.84751808553105E-15));
#22926=DIRECTION('',(1.,0.,0.));
#22927=DIRECTION('center_axis',(1.,0.,0.));
#22928=DIRECTION('ref_axis',(6.95715643956108E-17,1.,6.84751808553105E-15));
#22929=DIRECTION('',(1.,0.,0.));
#22930=DIRECTION('center_axis',(1.,0.,0.));
#22931=DIRECTION('ref_axis',(6.95715643956108E-17,1.,6.84751808553105E-15));
#22932=DIRECTION('',(1.,0.,0.));
#22933=DIRECTION('center_axis',(1.,0.,0.));
#22934=DIRECTION('ref_axis',(0.,0.,-1.));
#22935=DIRECTION('center_axis',(-1.,0.,0.));
#22936=DIRECTION('ref_axis',(0.,1.,0.));
#22937=DIRECTION('center_axis',(-1.,0.,0.));
#22938=DIRECTION('ref_axis',(0.,1.,0.));
#22939=DIRECTION('center_axis',(1.,0.,0.));
#22940=DIRECTION('ref_axis',(0.,0.,-1.));
#22941=DIRECTION('center_axis',(1.,0.,0.));
#22942=DIRECTION('ref_axis',(0.,1.,0.));
#22943=DIRECTION('center_axis',(1.,0.,0.));
#22944=DIRECTION('ref_axis',(0.,1.,0.));
#22945=DIRECTION('center_axis',(-1.,0.,0.));
#22946=DIRECTION('ref_axis',(6.95715643956108E-17,1.,6.84751808553105E-15));
#22947=DIRECTION('center_axis',(1.,0.,0.));
#22948=DIRECTION('ref_axis',(6.95715643956108E-17,1.,6.84751808553105E-15));
#22949=DIRECTION('center_axis',(0.,0.5,0.866025403784439));
#22950=DIRECTION('ref_axis',(0.,0.866025403784439,-0.5));
#22951=DIRECTION('',(0.,0.866025403784439,-0.5));
#22952=DIRECTION('',(-1.,0.,0.));
#22953=DIRECTION('',(0.,0.866025403784439,-0.5));
#22954=DIRECTION('',(-1.,0.,0.));
#22955=DIRECTION('center_axis',(0.,-0.5,0.866025403784439));
#22956=DIRECTION('ref_axis',(0.,0.866025403784439,0.5));
#22957=DIRECTION('',(0.,0.866025403784439,0.5));
#22958=DIRECTION('',(-1.,0.,0.));
#22959=DIRECTION('',(0.,0.866025403784439,0.5));
#22960=DIRECTION('center_axis',(0.,-1.,-1.92296268638356E-16));
#22961=DIRECTION('ref_axis',(0.,-1.92296268638356E-16,1.));
#22962=DIRECTION('',(0.,-1.92296268638356E-16,1.));
#22963=DIRECTION('',(-1.,0.,0.));
#22964=DIRECTION('',(0.,-1.92296268638356E-16,1.));
#22965=DIRECTION('center_axis',(0.,-0.5,-0.866025403784439));
#22966=DIRECTION('ref_axis',(0.,-0.866025403784439,0.5));
#22967=DIRECTION('',(0.,-0.866025403784439,0.5));
#22968=DIRECTION('',(-1.,0.,0.));
#22969=DIRECTION('',(0.,-0.866025403784439,0.5));
#22970=DIRECTION('center_axis',(0.,0.5,-0.866025403784439));
#22971=DIRECTION('ref_axis',(0.,-0.866025403784439,-0.5));
#22972=DIRECTION('',(0.,-0.866025403784439,-0.5));
#22973=DIRECTION('',(-1.,0.,0.));
#22974=DIRECTION('',(0.,-0.866025403784439,-0.5));
#22975=DIRECTION('center_axis',(0.,1.,-3.84592537276713E-16));
#22976=DIRECTION('ref_axis',(0.,-3.84592537276713E-16,-1.));
#22977=DIRECTION('',(0.,-3.84592537276713E-16,-1.));
#22978=DIRECTION('',(0.,-3.84592537276713E-16,-1.));
#22979=DIRECTION('center_axis',(-1.,0.,0.));
#22980=DIRECTION('ref_axis',(0.,0.,1.));
#22981=DIRECTION('center_axis',(-1.,0.,0.));
#22982=DIRECTION('ref_axis',(0.,0.,1.));
#22983=DIRECTION('center_axis',(1.,0.,0.));
#22984=DIRECTION('ref_axis',(0.,0.,-1.));
#22985=DIRECTION('center_axis',(1.,0.,0.));
#22986=DIRECTION('ref_axis',(0.,1.,0.));
#22987=DIRECTION('',(-0.707106781186548,0.707106781186547,8.65956056235493E-17));
#22988=DIRECTION('center_axis',(1.,0.,0.));
#22989=DIRECTION('ref_axis',(0.,1.,0.));
#22990=DIRECTION('center_axis',(-1.,0.,0.));
#22991=DIRECTION('ref_axis',(0.,1.,0.));
#22992=DIRECTION('center_axis',(-1.,0.,0.));
#22993=DIRECTION('ref_axis',(0.,1.,0.));
#22994=DIRECTION('center_axis',(1.,0.,0.));
#22995=DIRECTION('ref_axis',(0.,0.,-1.));
#22996=DIRECTION('',(-0.707106781186548,-0.707106781186547,-8.65956056235493E-17));
#22997=DIRECTION('center_axis',(1.,0.,0.));
#22998=DIRECTION('ref_axis',(0.,0.,-1.));
#22999=DIRECTION('axis',(0.,0.,1.));
#23000=DIRECTION('refdir',(1.,0.,0.));
#23001=DIRECTION('center_axis',(1.,0.,0.));
#23002=DIRECTION('ref_axis',(0.,1.,0.));
#23003=DIRECTION('',(-1.,0.,0.));
#23004=DIRECTION('center_axis',(1.,0.,0.));
#23005=DIRECTION('ref_axis',(0.,1.,0.));
#23006=DIRECTION('center_axis',(1.,0.,0.));
#23007=DIRECTION('ref_axis',(0.,1.,0.));
#23008=DIRECTION('',(-1.,0.,0.));
#23009=DIRECTION('center_axis',(1.,0.,0.));
#23010=DIRECTION('ref_axis',(0.,1.,0.));
#23011=DIRECTION('',(-1.,0.,0.));
#23012=DIRECTION('center_axis',(1.,0.,0.));
#23013=DIRECTION('ref_axis',(0.,1.,0.));
#23014=DIRECTION('',(-1.,0.,0.));
#23015=DIRECTION('center_axis',(1.,0.,0.));
#23016=DIRECTION('ref_axis',(0.,1.,0.));
#23017=DIRECTION('',(-1.,0.,0.));
#23018=DIRECTION('center_axis',(1.,0.,0.));
#23019=DIRECTION('ref_axis',(0.,1.,0.));
#23020=DIRECTION('',(-1.,0.,0.));
#23021=DIRECTION('center_axis',(1.,0.,0.));
#23022=DIRECTION('ref_axis',(0.,1.,0.));
#23023=DIRECTION('',(-1.,0.,0.));
#23024=DIRECTION('center_axis',(1.,0.,0.));
#23025=DIRECTION('ref_axis',(0.,1.,0.));
#23026=DIRECTION('',(-1.,0.,0.));
#23027=DIRECTION('center_axis',(1.,0.,0.));
#23028=DIRECTION('ref_axis',(0.,1.,0.));
#23029=DIRECTION('',(-1.,0.,0.));
#23030=DIRECTION('center_axis',(1.,0.,0.));
#23031=DIRECTION('ref_axis',(0.,1.,0.));
#23032=DIRECTION('',(-1.,0.,0.));
#23033=DIRECTION('center_axis',(1.,0.,0.));
#23034=DIRECTION('ref_axis',(0.,1.,0.));
#23035=DIRECTION('',(-1.,0.,0.));
#23036=DIRECTION('center_axis',(1.,0.,0.));
#23037=DIRECTION('ref_axis',(0.,1.,0.));
#23038=DIRECTION('',(-1.,0.,0.));
#23039=DIRECTION('center_axis',(1.,0.,0.));
#23040=DIRECTION('ref_axis',(0.,1.,0.));
#23041=DIRECTION('',(-1.,0.,0.));
#23042=DIRECTION('center_axis',(1.,0.,0.));
#23043=DIRECTION('ref_axis',(0.,1.,0.));
#23044=DIRECTION('',(-1.,0.,0.));
#23045=DIRECTION('center_axis',(1.,0.,0.));
#23046=DIRECTION('ref_axis',(0.,1.,0.));
#23047=DIRECTION('',(-1.,0.,0.));
#23048=DIRECTION('center_axis',(1.,0.,0.));
#23049=DIRECTION('ref_axis',(0.,0.960826707559551,-0.27714984762809));
#23050=DIRECTION('',(1.,0.,0.));
#23051=DIRECTION('center_axis',(1.,0.,0.));
#23052=DIRECTION('ref_axis',(0.,1.,9.63181083013289E-14));
#23053=DIRECTION('center_axis',(1.,0.,0.));
#23054=DIRECTION('ref_axis',(0.,1.,9.63181083013289E-14));
#23055=DIRECTION('',(1.,0.,0.));
#23056=DIRECTION('center_axis',(1.,0.,0.));
#23057=DIRECTION('ref_axis',(0.,1.,9.63181083013289E-14));
#23058=DIRECTION('',(1.,0.,0.));
#23059=DIRECTION('center_axis',(1.,0.,0.));
#23060=DIRECTION('ref_axis',(0.,1.,9.63181083013289E-14));
#23061=DIRECTION('',(1.,0.,0.));
#23062=DIRECTION('center_axis',(1.,0.,0.));
#23063=DIRECTION('ref_axis',(0.,1.,9.63181083013289E-14));
#23064=DIRECTION('',(1.,0.,0.));
#23065=DIRECTION('center_axis',(1.,0.,0.));
#23066=DIRECTION('ref_axis',(0.,1.,9.63181083013289E-14));
#23067=DIRECTION('',(1.,0.,0.));
#23068=DIRECTION('center_axis',(1.,0.,0.));
#23069=DIRECTION('ref_axis',(0.,1.,9.63181083013289E-14));
#23070=DIRECTION('',(1.,0.,0.));
#23071=DIRECTION('center_axis',(1.,0.,0.));
#23072=DIRECTION('ref_axis',(0.,1.,9.63181083013289E-14));
#23073=DIRECTION('',(1.,0.,0.));
#23074=DIRECTION('center_axis',(1.,0.,0.));
#23075=DIRECTION('ref_axis',(0.,1.,9.63181083013289E-14));
#23076=DIRECTION('',(1.,0.,0.));
#23077=DIRECTION('center_axis',(1.,0.,0.));
#23078=DIRECTION('ref_axis',(0.,1.,9.63181083013289E-14));
#23079=DIRECTION('',(1.,0.,0.));
#23080=DIRECTION('center_axis',(1.,0.,0.));
#23081=DIRECTION('ref_axis',(0.,1.,9.63181083013289E-14));
#23082=DIRECTION('',(1.,0.,0.));
#23083=DIRECTION('center_axis',(1.,0.,0.));
#23084=DIRECTION('ref_axis',(0.,1.,9.63181083013289E-14));
#23085=DIRECTION('',(1.,0.,0.));
#23086=DIRECTION('center_axis',(1.,0.,0.));
#23087=DIRECTION('ref_axis',(0.,1.,9.63181083013289E-14));
#23088=DIRECTION('',(1.,0.,0.));
#23089=DIRECTION('center_axis',(1.,0.,0.));
#23090=DIRECTION('ref_axis',(0.,1.,9.63181083013289E-14));
#23091=DIRECTION('',(1.,0.,0.));
#23092=DIRECTION('center_axis',(1.,0.,0.));
#23093=DIRECTION('ref_axis',(0.,0.,-1.));
#23094=DIRECTION('center_axis',(1.,0.,0.));
#23095=DIRECTION('ref_axis',(0.,1.,0.));
#23096=DIRECTION('center_axis',(1.,0.,0.));
#23097=DIRECTION('ref_axis',(0.,1.,0.));
#23098=DIRECTION('center_axis',(-1.,0.,0.));
#23099=DIRECTION('ref_axis',(0.,1.,9.63181083013289E-14));
#23100=DIRECTION('center_axis',(1.,0.,0.));
#23101=DIRECTION('ref_axis',(0.,1.,9.63181083013289E-14));
#23102=DIRECTION('center_axis',(0.,-0.499806704490841,0.866136974240221));
#23103=DIRECTION('ref_axis',(0.,-0.866136974240221,-0.499806704490841));
#23104=DIRECTION('',(1.,0.,0.));
#23105=DIRECTION('',(0.,-0.866136974240221,-0.499806704490841));
#23106=DIRECTION('',(-1.,0.,0.));
#23107=DIRECTION('center_axis',(1.,0.,0.));
#23108=DIRECTION('ref_axis',(0.,-0.20791169081776,-0.978147600733805));
#23109=DIRECTION('center_axis',(-1.,0.,0.));
#23110=DIRECTION('ref_axis',(0.,1.,0.));
#23111=DIRECTION('',(0.,0.587965797342076,-0.808885789933225));
#23112=DIRECTION('center_axis',(0.,-0.808885789933225,-0.587965797342076));
#23113=DIRECTION('ref_axis',(0.,0.587965797342076,-0.808885789933225));
#23114=DIRECTION('',(1.,0.,0.));
#23115=DIRECTION('center_axis',(1.,0.,0.));
#23116=DIRECTION('ref_axis',(0.,1.,0.));
#23117=DIRECTION('center_axis',(1.,0.,0.));
#23118=DIRECTION('ref_axis',(0.,0.,-1.));
#23119=DIRECTION('',(-1.,0.,0.));
#23120=DIRECTION('center_axis',(-1.,0.,0.));
#23121=DIRECTION('ref_axis',(0.,1.,0.));
#23122=DIRECTION('',(1.,0.,0.));
#23123=DIRECTION('center_axis',(1.,0.,0.));
#23124=DIRECTION('ref_axis',(0.,0.,-1.));
#23125=DIRECTION('',(-1.,0.,0.));
#23126=DIRECTION('center_axis',(-1.,0.,0.));
#23127=DIRECTION('ref_axis',(0.,1.,0.));
#23128=DIRECTION('',(1.,0.,0.));
#23129=DIRECTION('center_axis',(1.,0.,0.));
#23130=DIRECTION('ref_axis',(0.,0.,-1.));
#23131=DIRECTION('',(-1.,0.,0.));
#23132=DIRECTION('center_axis',(-1.,0.,0.));
#23133=DIRECTION('ref_axis',(0.,1.,0.));
#23134=DIRECTION('',(1.,0.,0.));
#23135=DIRECTION('center_axis',(1.,0.,0.));
#23136=DIRECTION('ref_axis',(0.,0.,-1.));
#23137=DIRECTION('',(-1.,0.,0.));
#23138=DIRECTION('center_axis',(-1.,0.,0.));
#23139=DIRECTION('ref_axis',(0.,1.,0.));
#23140=DIRECTION('',(1.,0.,0.));
#23141=DIRECTION('center_axis',(1.,0.,0.));
#23142=DIRECTION('ref_axis',(0.,0.,-1.));
#23143=DIRECTION('',(-1.,0.,0.));
#23144=DIRECTION('center_axis',(-1.,0.,0.));
#23145=DIRECTION('ref_axis',(0.,1.,0.));
#23146=DIRECTION('',(1.,0.,0.));
#23147=DIRECTION('center_axis',(1.,0.,0.));
#23148=DIRECTION('ref_axis',(0.,0.,-1.));
#23149=DIRECTION('',(-1.,0.,0.));
#23150=DIRECTION('center_axis',(-1.,0.,0.));
#23151=DIRECTION('ref_axis',(0.,1.,0.));
#23152=DIRECTION('',(1.,0.,0.));
#23153=DIRECTION('center_axis',(1.,0.,0.));
#23154=DIRECTION('ref_axis',(0.,0.,-1.));
#23155=DIRECTION('',(-1.,0.,0.));
#23156=DIRECTION('center_axis',(-1.,0.,0.));
#23157=DIRECTION('ref_axis',(0.,1.,0.));
#23158=DIRECTION('',(1.,0.,0.));
#23159=DIRECTION('center_axis',(1.,0.,0.));
#23160=DIRECTION('ref_axis',(0.,0.,-1.));
#23161=DIRECTION('',(-1.,0.,0.));
#23162=DIRECTION('center_axis',(-1.,0.,0.));
#23163=DIRECTION('ref_axis',(0.,1.,0.));
#23164=DIRECTION('',(1.,0.,0.));
#23165=DIRECTION('center_axis',(1.,0.,0.));
#23166=DIRECTION('ref_axis',(0.,0.,-1.));
#23167=DIRECTION('',(-1.,0.,0.));
#23168=DIRECTION('center_axis',(-1.,0.,0.));
#23169=DIRECTION('ref_axis',(0.,1.,0.));
#23170=DIRECTION('',(1.,0.,0.));
#23171=DIRECTION('center_axis',(1.,0.,0.));
#23172=DIRECTION('ref_axis',(0.,0.,-1.));
#23173=DIRECTION('',(-1.,0.,0.));
#23174=DIRECTION('center_axis',(-1.,0.,0.));
#23175=DIRECTION('ref_axis',(0.,1.,0.));
#23176=DIRECTION('',(1.,0.,0.));
#23177=DIRECTION('center_axis',(1.,0.,0.));
#23178=DIRECTION('ref_axis',(0.,0.,-1.));
#23179=DIRECTION('',(-1.,0.,0.));
#23180=DIRECTION('center_axis',(-1.,0.,0.));
#23181=DIRECTION('ref_axis',(0.,1.,0.));
#23182=DIRECTION('',(1.,0.,0.));
#23183=DIRECTION('center_axis',(1.,0.,0.));
#23184=DIRECTION('ref_axis',(0.,0.,-1.));
#23185=DIRECTION('',(-1.,0.,0.));
#23186=DIRECTION('center_axis',(-1.,0.,0.));
#23187=DIRECTION('ref_axis',(0.,1.,0.));
#23188=DIRECTION('',(1.,0.,0.));
#23189=DIRECTION('center_axis',(1.,0.,0.));
#23190=DIRECTION('ref_axis',(0.,0.,-1.));
#23191=DIRECTION('',(-1.,0.,0.));
#23192=DIRECTION('center_axis',(-1.,0.,0.));
#23193=DIRECTION('ref_axis',(0.,1.,0.));
#23194=DIRECTION('',(1.,0.,0.));
#23195=DIRECTION('center_axis',(1.,0.,0.));
#23196=DIRECTION('ref_axis',(0.,0.,-1.));
#23197=DIRECTION('',(-1.,0.,0.));
#23198=DIRECTION('center_axis',(-1.,0.,0.));
#23199=DIRECTION('ref_axis',(0.,1.,0.));
#23200=DIRECTION('',(-1.,0.,0.));
#23201=DIRECTION('center_axis',(1.,0.,0.));
#23202=DIRECTION('ref_axis',(0.,0.,-1.));
#23203=DIRECTION('center_axis',(-1.,0.,0.));
#23204=DIRECTION('ref_axis',(0.,1.,0.));
#23205=DIRECTION('',(1.,0.,0.));
#23206=DIRECTION('center_axis',(1.,0.,0.));
#23207=DIRECTION('ref_axis',(0.,0.,-1.));
#23208=DIRECTION('',(-1.,0.,0.));
#23209=DIRECTION('center_axis',(-1.,0.,0.));
#23210=DIRECTION('ref_axis',(0.,1.,0.));
#23211=DIRECTION('',(1.,0.,0.));
#23212=DIRECTION('center_axis',(1.,0.,0.));
#23213=DIRECTION('ref_axis',(0.,0.,-1.));
#23214=DIRECTION('',(-1.,0.,0.));
#23215=DIRECTION('center_axis',(-1.,0.,0.));
#23216=DIRECTION('ref_axis',(0.,1.,0.));
#23217=DIRECTION('',(1.,0.,0.));
#23218=DIRECTION('center_axis',(1.,0.,0.));
#23219=DIRECTION('ref_axis',(0.,0.,-1.));
#23220=DIRECTION('',(-1.,0.,0.));
#23221=DIRECTION('center_axis',(-1.,0.,0.));
#23222=DIRECTION('ref_axis',(0.,1.,0.));
#23223=DIRECTION('',(1.,0.,0.));
#23224=DIRECTION('center_axis',(1.,0.,0.));
#23225=DIRECTION('ref_axis',(0.,0.,-1.));
#23226=DIRECTION('',(-1.,0.,0.));
#23227=DIRECTION('center_axis',(-1.,0.,0.));
#23228=DIRECTION('ref_axis',(0.,1.,0.));
#23229=DIRECTION('',(1.,0.,0.));
#23230=DIRECTION('center_axis',(1.,0.,0.));
#23231=DIRECTION('ref_axis',(0.,0.,-1.));
#23232=DIRECTION('',(-1.,0.,0.));
#23233=DIRECTION('center_axis',(-1.,0.,0.));
#23234=DIRECTION('ref_axis',(0.,1.,0.));
#23235=DIRECTION('',(1.,0.,0.));
#23236=DIRECTION('center_axis',(1.,0.,0.));
#23237=DIRECTION('ref_axis',(0.,0.,-1.));
#23238=DIRECTION('',(-1.,0.,0.));
#23239=DIRECTION('center_axis',(-1.,0.,0.));
#23240=DIRECTION('ref_axis',(0.,1.,0.));
#23241=DIRECTION('',(1.,0.,0.));
#23242=DIRECTION('center_axis',(1.,0.,0.));
#23243=DIRECTION('ref_axis',(0.,0.,-1.));
#23244=DIRECTION('',(-1.,0.,0.));
#23245=DIRECTION('center_axis',(-1.,0.,0.));
#23246=DIRECTION('ref_axis',(0.,1.,0.));
#23247=DIRECTION('',(1.,0.,0.));
#23248=DIRECTION('center_axis',(1.,0.,0.));
#23249=DIRECTION('ref_axis',(0.,0.,-1.));
#23250=DIRECTION('',(-1.,0.,0.));
#23251=DIRECTION('center_axis',(-1.,0.,0.));
#23252=DIRECTION('ref_axis',(0.,1.,0.));
#23253=DIRECTION('',(1.,0.,0.));
#23254=DIRECTION('center_axis',(1.,0.,0.));
#23255=DIRECTION('ref_axis',(0.,0.,-1.));
#23256=DIRECTION('',(-1.,0.,0.));
#23257=DIRECTION('center_axis',(-1.,0.,0.));
#23258=DIRECTION('ref_axis',(0.,1.,0.));
#23259=DIRECTION('',(1.,0.,0.));
#23260=DIRECTION('center_axis',(1.,0.,0.));
#23261=DIRECTION('ref_axis',(0.,0.,-1.));
#23262=DIRECTION('',(-1.,0.,0.));
#23263=DIRECTION('center_axis',(-1.,0.,0.));
#23264=DIRECTION('ref_axis',(0.,1.,0.));
#23265=DIRECTION('',(1.,0.,0.));
#23266=DIRECTION('center_axis',(1.,0.,0.));
#23267=DIRECTION('ref_axis',(0.,0.,-1.));
#23268=DIRECTION('',(-1.,0.,0.));
#23269=DIRECTION('center_axis',(-1.,0.,0.));
#23270=DIRECTION('ref_axis',(0.,1.,0.));
#23271=DIRECTION('',(1.,0.,0.));
#23272=DIRECTION('center_axis',(1.,0.,0.));
#23273=DIRECTION('ref_axis',(0.,0.,-1.));
#23274=DIRECTION('',(-1.,0.,0.));
#23275=DIRECTION('center_axis',(-1.,0.,0.));
#23276=DIRECTION('ref_axis',(0.,1.,0.));
#23277=DIRECTION('',(1.,0.,0.));
#23278=DIRECTION('center_axis',(1.,0.,0.));
#23279=DIRECTION('ref_axis',(0.,0.,-1.));
#23280=DIRECTION('',(-1.,0.,0.));
#23281=DIRECTION('center_axis',(-1.,0.,0.));
#23282=DIRECTION('ref_axis',(0.,1.,0.));
#23283=DIRECTION('',(1.,0.,0.));
#23284=DIRECTION('center_axis',(1.,0.,0.));
#23285=DIRECTION('ref_axis',(0.,0.,-1.));
#23286=DIRECTION('',(-1.,0.,0.));
#23287=DIRECTION('center_axis',(-1.,0.,0.));
#23288=DIRECTION('ref_axis',(0.,1.,0.));
#23289=DIRECTION('',(1.,0.,0.));
#23290=DIRECTION('center_axis',(1.,0.,0.));
#23291=DIRECTION('ref_axis',(0.,0.,-1.));
#23292=DIRECTION('',(-1.,0.,0.));
#23293=DIRECTION('center_axis',(-1.,0.,0.));
#23294=DIRECTION('ref_axis',(0.,1.,0.));
#23295=DIRECTION('',(1.,0.,0.));
#23296=DIRECTION('center_axis',(1.,0.,0.));
#23297=DIRECTION('ref_axis',(0.,0.,-1.));
#23298=DIRECTION('center_axis',(0.,-0.308804726034324,0.951125460272653));
#23299=DIRECTION('ref_axis',(0.,-0.951125460272653,-0.308804726034324));
#23300=DIRECTION('',(1.,0.,0.));
#23301=DIRECTION('',(0.,-0.951125460272653,-0.308804726034324));
#23302=DIRECTION('center_axis',(1.,0.,0.));
#23303=DIRECTION('ref_axis',(0.,-0.406736643075801,-0.913545457642601));
#23304=DIRECTION('',(0.,0.406940521720215,-0.913454657759256));
#23305=DIRECTION('center_axis',(0.,-0.913454657759256,-0.406940521720215));
#23306=DIRECTION('ref_axis',(0.,0.406940521720215,-0.913454657759256));
#23307=DIRECTION('center_axis',(0.,-0.104306499240628,0.994545199684843));
#23308=DIRECTION('ref_axis',(0.,-0.994545199684843,-0.104306499240628));
#23309=DIRECTION('',(1.,0.,0.));
#23310=DIRECTION('',(0.,-0.994545199684843,-0.104306499240628));
#23311=DIRECTION('center_axis',(1.,0.,0.));
#23312=DIRECTION('ref_axis',(0.,-0.587785252292473,-0.809016994374947));
#23313=DIRECTION('',(0.,0.208129992581907,-0.978101173799447));
#23314=DIRECTION('center_axis',(0.,-0.978101173799447,-0.208129992581907));
#23315=DIRECTION('ref_axis',(0.,0.208129992581907,-0.978101173799447));
#23316=DIRECTION('center_axis',(0.,0.104750422088,0.994498541513454));
#23317=DIRECTION('ref_axis',(0.,-0.994498541513453,0.104750422088));
#23318=DIRECTION('',(1.,0.,0.));
#23319=DIRECTION('',(0.,-0.994498541513453,0.104750422088));
#23320=DIRECTION('center_axis',(1.,0.,0.));
#23321=DIRECTION('ref_axis',(0.,-0.743144825477395,-0.669130606358858));
#23322=DIRECTION('',(0.,0.000223184049258973,-0.99999997509444));
#23323=DIRECTION('center_axis',(0.,-0.99999997509444,-0.000223184049258973));
#23324=DIRECTION('ref_axis',(0.,0.000223184049258973,-0.99999997509444));
#23325=DIRECTION('center_axis',(0.,0.309229247323088,0.950987524944463));
#23326=DIRECTION('ref_axis',(0.,-0.950987524944463,0.309229247323088));
#23327=DIRECTION('',(1.,0.,0.));
#23328=DIRECTION('',(0.,-0.950987524944463,0.309229247323088));
#23329=DIRECTION('center_axis',(1.,0.,0.));
#23330=DIRECTION('ref_axis',(0.,-0.866025403784439,-0.499999999999999));
#23331=DIRECTION('',(0.,-0.207693378697298,-0.978193978945537));
#23332=DIRECTION('center_axis',(0.,-0.978193978945537,0.207693378697298));
#23333=DIRECTION('ref_axis',(0.,-0.207693378697298,-0.978193978945537));
#23334=DIRECTION('center_axis',(0.,0.500193270603598,0.865913790190961));
#23335=DIRECTION('ref_axis',(0.,-0.865913790190961,0.500193270603598));
#23336=DIRECTION('',(1.,0.,0.));
#23337=DIRECTION('',(0.,-0.865913790190961,0.500193270603598));
#23338=DIRECTION('center_axis',(1.,0.,0.));
#23339=DIRECTION('ref_axis',(0.,-0.951056516295154,-0.309016994374947));
#23340=DIRECTION('',(0.,-0.406532744171377,-0.913636212021223));
#23341=DIRECTION('center_axis',(0.,-0.913636212021223,0.406532744171377));
#23342=DIRECTION('ref_axis',(0.,-0.406532744171377,-0.913636212021223));
#23343=DIRECTION('center_axis',(0.,0.669296447765122,0.742995467690745));
#23344=DIRECTION('ref_axis',(0.,-0.742995467690745,0.669296447765122));
#23345=DIRECTION('',(1.,0.,0.));
#23346=DIRECTION('',(0.,-0.742995467690745,0.669296447765122));
#23347=DIRECTION('center_axis',(1.,0.,0.));
#23348=DIRECTION('ref_axis',(0.,-0.994521895368273,-0.104528463267653));
#23349=DIRECTION('',(0.,-0.587604677964628,-0.809148158518627));
#23350=DIRECTION('center_axis',(0.,-0.809148158518627,0.587604677964628));
#23351=DIRECTION('ref_axis',(0.,-0.587604677964628,-0.809148158518627));
#23352=DIRECTION('center_axis',(0.,0.809148158518628,0.587604677964627));
#23353=DIRECTION('ref_axis',(0.,-0.587604677964627,0.809148158518628));
#23354=DIRECTION('',(1.,0.,0.));
#23355=DIRECTION('',(0.,-0.587604677964627,0.809148158518628));
#23356=DIRECTION('center_axis',(1.,0.,0.));
#23357=DIRECTION('ref_axis',(0.,-0.994521895368273,0.104528463267654));
#23358=DIRECTION('',(0.,-0.742995467690746,-0.669296447765121));
#23359=DIRECTION('center_axis',(0.,-0.669296447765121,0.742995467690746));
#23360=DIRECTION('ref_axis',(0.,-0.742995467690746,-0.669296447765121));
#23361=DIRECTION('center_axis',(0.,0.913636212021223,0.406532744171377));
#23362=DIRECTION('ref_axis',(0.,-0.406532744171377,0.913636212021223));
#23363=DIRECTION('',(1.,0.,0.));
#23364=DIRECTION('',(0.,-0.406532744171377,0.913636212021223));
#23365=DIRECTION('center_axis',(1.,0.,0.));
#23366=DIRECTION('ref_axis',(0.,-0.951056516295153,0.309016994374948));
#23367=DIRECTION('',(0.,-0.865913790190961,-0.500193270603598));
#23368=DIRECTION('center_axis',(0.,-0.500193270603598,0.865913790190961));
#23369=DIRECTION('ref_axis',(0.,-0.865913790190961,-0.500193270603598));
#23370=DIRECTION('center_axis',(0.,0.978193978945537,0.207693378697297));
#23371=DIRECTION('ref_axis',(0.,-0.207693378697296,0.978193978945537));
#23372=DIRECTION('',(1.,0.,0.));
#23373=DIRECTION('',(0.,-0.207693378697296,0.978193978945537));
#23374=DIRECTION('center_axis',(1.,0.,0.));
#23375=DIRECTION('ref_axis',(0.,-0.866025403784438,0.5));
#23376=DIRECTION('',(0.,-0.950987524944464,-0.309229247323087));
#23377=DIRECTION('center_axis',(0.,-0.309229247323087,0.950987524944464));
#23378=DIRECTION('ref_axis',(0.,-0.950987524944464,-0.309229247323087));
#23379=DIRECTION('center_axis',(0.,0.99999997509444,-0.000223184049259806));
#23380=DIRECTION('ref_axis',(0.,0.000223184049259806,0.99999997509444));
#23381=DIRECTION('',(1.,0.,0.));
#23382=DIRECTION('',(0.,0.000223184049259806,0.99999997509444));
#23383=DIRECTION('center_axis',(1.,0.,0.));
#23384=DIRECTION('ref_axis',(0.,-0.743144825477394,0.669130606358858));
#23385=DIRECTION('',(0.,-0.994498541513453,-0.104750422087999));
#23386=DIRECTION('center_axis',(0.,-0.104750422087999,0.994498541513454));
#23387=DIRECTION('ref_axis',(0.,-0.994498541513453,-0.104750422087999));
#23388=DIRECTION('center_axis',(0.,0.978101173799447,-0.208129992581908));
#23389=DIRECTION('ref_axis',(0.,0.208129992581907,0.978101173799446));
#23390=DIRECTION('',(1.,0.,0.));
#23391=DIRECTION('',(0.,0.208129992581907,0.978101173799446));
#23392=DIRECTION('center_axis',(1.,0.,0.));
#23393=DIRECTION('ref_axis',(0.,-0.587785252292473,0.809016994374947));
#23394=DIRECTION('',(0.,-0.994545199684843,0.104306499240628));
#23395=DIRECTION('center_axis',(0.,0.104306499240628,0.994545199684843));
#23396=DIRECTION('ref_axis',(0.,-0.994545199684843,0.104306499240628));
#23397=DIRECTION('center_axis',(0.,0.913454657759255,-0.406940521720216));
#23398=DIRECTION('ref_axis',(0.,0.406940521720216,0.913454657759255));
#23399=DIRECTION('',(1.,0.,0.));
#23400=DIRECTION('',(0.,0.406940521720216,0.913454657759255));
#23401=DIRECTION('center_axis',(1.,0.,0.));
#23402=DIRECTION('ref_axis',(0.,-0.4067366430758,0.913545457642601));
#23403=DIRECTION('',(0.,-0.951125460272653,0.308804726034325));
#23404=DIRECTION('center_axis',(0.,0.308804726034325,0.951125460272653));
#23405=DIRECTION('ref_axis',(0.,-0.951125460272653,0.308804726034325));
#23406=DIRECTION('center_axis',(0.,0.808885789933224,-0.587965797342077));
#23407=DIRECTION('ref_axis',(0.,0.587965797342077,0.808885789933224));
#23408=DIRECTION('',(1.,0.,0.));
#23409=DIRECTION('',(0.,0.587965797342077,0.808885789933224));
#23410=DIRECTION('center_axis',(1.,0.,0.));
#23411=DIRECTION('ref_axis',(0.,-0.207911690817759,0.978147600733806));
#23412=DIRECTION('',(0.,-0.86613697424022,0.499806704490842));
#23413=DIRECTION('center_axis',(0.,0.499806704490842,0.86613697424022));
#23414=DIRECTION('ref_axis',(0.,-0.86613697424022,0.499806704490842));
#23415=DIRECTION('center_axis',(0.,0.668964731622449,-0.743294146247167));
#23416=DIRECTION('ref_axis',(0.,0.743294146247167,0.668964731622449));
#23417=DIRECTION('',(1.,0.,0.));
#23418=DIRECTION('',(0.,0.743294146247167,0.668964731622449));
#23419=DIRECTION('center_axis',(1.,0.,0.));
#23420=DIRECTION('ref_axis',(0.,1.22464679914735E-16,1.));
#23421=DIRECTION('',(0.,-0.743294146247166,0.668964731622449));
#23422=DIRECTION('center_axis',(0.,0.66896473162245,0.743294146247167));
#23423=DIRECTION('ref_axis',(0.,-0.743294146247166,0.668964731622449));
#23424=DIRECTION('center_axis',(0.,0.499806704490841,-0.866136974240221));
#23425=DIRECTION('ref_axis',(0.,0.866136974240221,0.499806704490841));
#23426=DIRECTION('',(1.,0.,0.));
#23427=DIRECTION('',(0.,0.866136974240221,0.499806704490841));
#23428=DIRECTION('center_axis',(1.,0.,0.));
#23429=DIRECTION('ref_axis',(0.,0.20791169081776,0.978147600733805));
#23430=DIRECTION('',(0.,-0.587965797342076,0.808885789933224));
#23431=DIRECTION('center_axis',(0.,0.808885789933225,0.587965797342076));
#23432=DIRECTION('ref_axis',(0.,-0.587965797342076,0.808885789933224));
#23433=DIRECTION('center_axis',(0.,0.308804726034324,-0.951125460272653));
#23434=DIRECTION('ref_axis',(0.,0.951125460272653,0.308804726034324));
#23435=DIRECTION('',(1.,0.,0.));
#23436=DIRECTION('',(0.,0.951125460272653,0.308804726034324));
#23437=DIRECTION('center_axis',(1.,0.,0.));
#23438=DIRECTION('ref_axis',(0.,0.4067366430758,0.913545457642601));
#23439=DIRECTION('',(0.,-0.406940521720215,0.913454657759256));
#23440=DIRECTION('center_axis',(0.,0.913454657759256,0.406940521720215));
#23441=DIRECTION('ref_axis',(0.,-0.406940521720215,0.913454657759256));
#23442=DIRECTION('center_axis',(0.,0.104306499240628,-0.994545199684843));
#23443=DIRECTION('ref_axis',(0.,0.994545199684843,0.104306499240628));
#23444=DIRECTION('',(1.,0.,0.));
#23445=DIRECTION('',(0.,0.994545199684843,0.104306499240628));
#23446=DIRECTION('center_axis',(1.,0.,0.));
#23447=DIRECTION('ref_axis',(0.,0.587785252292473,0.809016994374947));
#23448=DIRECTION('',(0.,-0.208129992581907,0.978101173799447));
#23449=DIRECTION('center_axis',(0.,0.978101173799447,0.208129992581907));
#23450=DIRECTION('ref_axis',(0.,-0.208129992581907,0.978101173799447));
#23451=DIRECTION('center_axis',(0.,-0.104750422087999,-0.994498541513453));
#23452=DIRECTION('ref_axis',(0.,0.994498541513453,-0.104750422087999));
#23453=DIRECTION('',(1.,0.,0.));
#23454=DIRECTION('',(0.,0.994498541513453,-0.104750422087999));
#23455=DIRECTION('center_axis',(1.,0.,0.));
#23456=DIRECTION('ref_axis',(0.,0.743144825477394,0.669130606358858));
#23457=DIRECTION('',(0.,-0.000223184049259084,0.99999997509444));
#23458=DIRECTION('center_axis',(0.,0.99999997509444,0.000223184049259084));
#23459=DIRECTION('ref_axis',(0.,-0.000223184049259084,0.99999997509444));
#23460=DIRECTION('center_axis',(0.,-0.309229247323088,-0.950987524944464));
#23461=DIRECTION('ref_axis',(0.,0.950987524944463,-0.309229247323088));
#23462=DIRECTION('',(1.,0.,0.));
#23463=DIRECTION('',(0.,0.950987524944463,-0.309229247323088));
#23464=DIRECTION('center_axis',(1.,0.,0.));
#23465=DIRECTION('ref_axis',(0.,0.866025403784439,0.5));
#23466=DIRECTION('',(0.,0.207693378697297,0.978193978945537));
#23467=DIRECTION('center_axis',(0.,0.978193978945537,-0.207693378697297));
#23468=DIRECTION('ref_axis',(0.,0.207693378697297,0.978193978945537));
#23469=DIRECTION('center_axis',(0.,-0.500193270603598,-0.865913790190961));
#23470=DIRECTION('ref_axis',(0.,0.865913790190961,-0.500193270603598));
#23471=DIRECTION('',(1.,0.,0.));
#23472=DIRECTION('',(0.,0.865913790190961,-0.500193270603598));
#23473=DIRECTION('center_axis',(1.,0.,0.));
#23474=DIRECTION('ref_axis',(0.,0.951056516295154,0.309016994374947));
#23475=DIRECTION('',(0.,0.406532744171377,0.913636212021223));
#23476=DIRECTION('center_axis',(0.,0.913636212021223,-0.406532744171377));
#23477=DIRECTION('ref_axis',(0.,0.406532744171377,0.913636212021223));
#23478=DIRECTION('center_axis',(0.,-0.669296447765122,-0.742995467690745));
#23479=DIRECTION('ref_axis',(0.,0.742995467690745,-0.669296447765122));
#23480=DIRECTION('',(1.,0.,0.));
#23481=DIRECTION('',(0.,0.742995467690745,-0.669296447765122));
#23482=DIRECTION('center_axis',(1.,0.,0.));
#23483=DIRECTION('ref_axis',(0.,0.994521895368273,0.104528463267653));
#23484=DIRECTION('',(0.,0.587604677964628,0.809148158518628));
#23485=DIRECTION('center_axis',(0.,0.809148158518628,-0.587604677964628));
#23486=DIRECTION('ref_axis',(0.,0.587604677964628,0.809148158518628));
#23487=DIRECTION('center_axis',(0.,-0.809148158518628,-0.587604677964628));
#23488=DIRECTION('ref_axis',(0.,0.587604677964628,-0.809148158518628));
#23489=DIRECTION('',(1.,0.,0.));
#23490=DIRECTION('',(0.,0.587604677964628,-0.809148158518628));
#23491=DIRECTION('center_axis',(1.,0.,0.));
#23492=DIRECTION('ref_axis',(0.,0.994521895368273,-0.104528463267654));
#23493=DIRECTION('',(0.,0.742995467690746,0.669296447765122));
#23494=DIRECTION('center_axis',(0.,0.669296447765122,-0.742995467690746));
#23495=DIRECTION('ref_axis',(0.,0.742995467690746,0.669296447765122));
#23496=DIRECTION('center_axis',(0.,-0.913636212021223,-0.406532744171377));
#23497=DIRECTION('ref_axis',(0.,0.406532744171377,-0.913636212021223));
#23498=DIRECTION('',(1.,0.,0.));
#23499=DIRECTION('',(0.,0.406532744171377,-0.913636212021223));
#23500=DIRECTION('center_axis',(1.,0.,0.));
#23501=DIRECTION('ref_axis',(0.,0.951056516295154,-0.309016994374948));
#23502=DIRECTION('',(0.,0.865913790190961,0.500193270603598));
#23503=DIRECTION('center_axis',(0.,0.500193270603598,-0.865913790190961));
#23504=DIRECTION('ref_axis',(0.,0.865913790190961,0.500193270603598));
#23505=DIRECTION('center_axis',(0.,-0.978193978945537,-0.207693378697297));
#23506=DIRECTION('ref_axis',(0.,0.207693378697297,-0.978193978945537));
#23507=DIRECTION('',(1.,0.,0.));
#23508=DIRECTION('',(0.,0.207693378697297,-0.978193978945537));
#23509=DIRECTION('center_axis',(1.,0.,0.));
#23510=DIRECTION('ref_axis',(0.,0.866025403784439,-0.5));
#23511=DIRECTION('',(0.,0.950987524944464,0.309229247323087));
#23512=DIRECTION('center_axis',(0.,0.309229247323087,-0.950987524944464));
#23513=DIRECTION('ref_axis',(0.,0.950987524944464,0.309229247323087));
#23514=DIRECTION('center_axis',(0.,-0.99999997509444,0.000223184049259584));
#23515=DIRECTION('ref_axis',(0.,-0.000223184049259584,-0.99999997509444));
#23516=DIRECTION('',(1.,0.,0.));
#23517=DIRECTION('',(0.,-0.000223184049259584,-0.99999997509444));
#23518=DIRECTION('center_axis',(1.,0.,0.));
#23519=DIRECTION('ref_axis',(0.,0.743144825477394,-0.669130606358858));
#23520=DIRECTION('',(0.,0.994498541513454,0.104750422087999));
#23521=DIRECTION('center_axis',(0.,0.104750422087999,-0.994498541513454));
#23522=DIRECTION('ref_axis',(0.,0.994498541513454,0.104750422087999));
#23523=DIRECTION('center_axis',(0.,-0.978101173799447,0.208129992581907));
#23524=DIRECTION('ref_axis',(0.,-0.208129992581907,-0.978101173799446));
#23525=DIRECTION('',(1.,0.,0.));
#23526=DIRECTION('',(0.,-0.208129992581907,-0.978101173799446));
#23527=DIRECTION('center_axis',(1.,0.,0.));
#23528=DIRECTION('ref_axis',(0.,0.587785252292473,-0.809016994374947));
#23529=DIRECTION('',(0.,0.994545199684843,-0.104306499240628));
#23530=DIRECTION('center_axis',(0.,-0.104306499240628,-0.994545199684843));
#23531=DIRECTION('ref_axis',(0.,0.994545199684843,-0.104306499240628));
#23532=DIRECTION('center_axis',(0.,-0.913454657759256,0.406940521720216));
#23533=DIRECTION('ref_axis',(0.,-0.406940521720215,-0.913454657759256));
#23534=DIRECTION('',(1.,0.,0.));
#23535=DIRECTION('',(0.,-0.406940521720215,-0.913454657759256));
#23536=DIRECTION('center_axis',(1.,0.,0.));
#23537=DIRECTION('ref_axis',(0.,0.4067366430758,-0.913545457642601));
#23538=DIRECTION('',(0.,0.951125460272653,-0.308804726034325));
#23539=DIRECTION('center_axis',(0.,-0.308804726034325,-0.951125460272653));
#23540=DIRECTION('ref_axis',(0.,0.951125460272653,-0.308804726034325));
#23541=DIRECTION('center_axis',(0.,-0.808885789933224,0.587965797342076));
#23542=DIRECTION('ref_axis',(0.,-0.587965797342076,-0.808885789933224));
#23543=DIRECTION('',(1.,0.,0.));
#23544=DIRECTION('',(0.,-0.587965797342076,-0.808885789933224));
#23545=DIRECTION('center_axis',(1.,0.,0.));
#23546=DIRECTION('ref_axis',(0.,0.207911690817759,-0.978147600733806));
#23547=DIRECTION('',(0.,0.866136974240221,-0.499806704490842));
#23548=DIRECTION('center_axis',(0.,-0.499806704490842,-0.866136974240221));
#23549=DIRECTION('ref_axis',(0.,0.866136974240221,-0.499806704490842));
#23550=DIRECTION('center_axis',(0.,-0.668964731622449,0.743294146247167));
#23551=DIRECTION('ref_axis',(0.,-0.743294146247167,-0.668964731622449));
#23552=DIRECTION('',(1.,0.,0.));
#23553=DIRECTION('',(0.,-0.743294146247167,-0.668964731622449));
#23554=DIRECTION('center_axis',(1.,0.,0.));
#23555=DIRECTION('ref_axis',(0.,0.,-1.));
#23556=DIRECTION('',(0.,0.743294146247167,-0.668964731622449));
#23557=DIRECTION('center_axis',(0.,-0.668964731622449,-0.743294146247167));
#23558=DIRECTION('ref_axis',(0.,0.743294146247167,-0.668964731622449));
#23559=DIRECTION('center_axis',(-1.,0.,0.));
#23560=DIRECTION('ref_axis',(0.,0.,1.));
#23561=DIRECTION('center_axis',(1.,0.,0.));
#23562=DIRECTION('ref_axis',(0.,0.,-1.));
#23563=DIRECTION('center_axis',(1.,0.,0.));
#23564=DIRECTION('ref_axis',(0.,1.,0.));
#23565=DIRECTION('',(-0.707106781186548,0.707106781186547,8.65956056235493E-17));
#23566=DIRECTION('center_axis',(1.,0.,0.));
#23567=DIRECTION('ref_axis',(0.,1.,0.));
#23568=DIRECTION('center_axis',(1.,0.,0.));
#23569=DIRECTION('ref_axis',(0.,1.,0.));
#23570=DIRECTION('center_axis',(-1.,0.,0.));
#23571=DIRECTION('ref_axis',(0.,0.,1.));
#23572=DIRECTION('center_axis',(1.,0.,0.));
#23573=DIRECTION('ref_axis',(0.,0.,-1.));
#23574=DIRECTION('center_axis',(1.,0.,0.));
#23575=DIRECTION('ref_axis',(0.,1.,0.));
#23576=DIRECTION('',(-0.707106781186548,0.707106781186547,8.65956056235493E-17));
#23577=DIRECTION('center_axis',(-1.,0.,0.));
#23578=DIRECTION('ref_axis',(0.,1.,0.));
#23579=DIRECTION('center_axis',(1.,0.,0.));
#23580=DIRECTION('ref_axis',(0.,0.,-1.));
#23581=DIRECTION('',(-0.707106781186548,-0.707106781186547,-8.65956056235493E-17));
#23582=DIRECTION('center_axis',(1.,0.,0.));
#23583=DIRECTION('ref_axis',(0.,0.,-1.));
#23584=DIRECTION('',(0.,0.,1.));
#23585=DIRECTION('',(1.,0.,0.));
#23586=DIRECTION('',(0.,0.,1.));
#23587=DIRECTION('',(1.,0.,0.));
#23588=DIRECTION('',(-1.,-5.55111512312578E-17,0.));
#23589=DIRECTION('',(0.,0.,1.));
#23590=DIRECTION('',(-1.,-5.55111512312578E-17,0.));
#23591=DIRECTION('',(0.,0.,1.));
#23592=DIRECTION('',(-1.,-5.55111512312578E-17,0.));
#23593=DIRECTION('',(0.,0.,1.));
#23594=DIRECTION('',(-1.,-5.55111512312578E-17,0.));
#23595=DIRECTION('',(0.,0.,1.));
#23596=DIRECTION('',(-1.,-5.55111512312578E-17,0.));
#23597=DIRECTION('',(0.,0.,1.));
#23598=DIRECTION('',(-1.,0.,0.));
#23599=DIRECTION('',(0.,0.,1.));
#23600=DIRECTION('',(-1.,-5.55111512312578E-17,0.));
#23601=DIRECTION('',(0.,0.,1.));
#23602=DIRECTION('',(-1.,0.,0.));
#23603=DIRECTION('',(0.,0.,1.));
#23604=DIRECTION('',(-1.,0.,0.));
#23605=DIRECTION('',(0.,0.,1.));
#23606=DIRECTION('',(-1.,0.,0.));
#23607=DIRECTION('',(0.,0.,1.));
#23608=DIRECTION('',(-1.,0.,0.));
#23609=DIRECTION('',(0.,0.,1.));
#23610=DIRECTION('',(-1.,0.,0.));
#23611=DIRECTION('',(0.,0.,1.));
#23612=DIRECTION('',(1.,0.,0.));
#23613=DIRECTION('',(0.,0.,-1.));
#23614=DIRECTION('',(0.,0.,-1.));
#23615=DIRECTION('',(0.,1.,0.));
#23616=CARTESIAN_POINT('',(0.,0.,0.));
#23617=CARTESIAN_POINT('',(0.,0.,0.));
#23618=CARTESIAN_POINT('Origin',(-51.5,17.25,9.75));
#23619=CARTESIAN_POINT('',(-51.5,17.5,10.));
#23620=CARTESIAN_POINT('',(-63.5,17.5,10.));
#23621=CARTESIAN_POINT('',(-51.5,17.5,10.));
#23622=CARTESIAN_POINT('',(-63.,17.,9.5));
#23623=CARTESIAN_POINT('',(-63.5,17.5,10.));
#23624=CARTESIAN_POINT('',(-52.,17.,9.5));
#23625=CARTESIAN_POINT('',(-51.5,17.,9.5));
#23626=CARTESIAN_POINT('',(-51.5,17.5,10.));
#23627=CARTESIAN_POINT('Origin',(-46.,1.75,9.75));
#23628=CARTESIAN_POINT('',(-63.5,1.5,10.));
#23629=CARTESIAN_POINT('',(-51.5,1.5,10.));
#23630=CARTESIAN_POINT('',(-46.,1.5,10.));
#23631=CARTESIAN_POINT('',(-52.,2.,9.5));
#23632=CARTESIAN_POINT('',(-51.5,1.5,10.));
#23633=CARTESIAN_POINT('',(-63.,2.,9.5));
#23634=CARTESIAN_POINT('',(-46.,2.,9.5));
#23635=CARTESIAN_POINT('',(-63.,2.,9.5));
#23636=CARTESIAN_POINT('Origin',(-51.75,-2.5,9.75));
#23637=CARTESIAN_POINT('',(-52.,-2.5,9.5));
#23638=CARTESIAN_POINT('',(-51.5,-2.5,10.));
#23639=CARTESIAN_POINT('Origin',(-63.25,-10.,9.75));
#23640=CARTESIAN_POINT('',(-63.5,-10.,10.));
#23641=CARTESIAN_POINT('',(-63.,-10.,9.5));
#23642=CARTESIAN_POINT('Origin',(-63.,2.,10.));
#23643=CARTESIAN_POINT('',(-63.,2.,4.));
#23644=CARTESIAN_POINT('',(-63.,2.,10.));
#23645=CARTESIAN_POINT('',(-63.,17.,4.));
#23646=CARTESIAN_POINT('',(-63.,17.,4.));
#23647=CARTESIAN_POINT('',(-63.,17.,10.));
#23648=CARTESIAN_POINT('Origin',(-52.,2.,10.));
#23649=CARTESIAN_POINT('',(-52.,2.,4.));
#23650=CARTESIAN_POINT('',(-52.,2.,10.));
#23651=CARTESIAN_POINT('',(-63.,2.,4.));
#23652=CARTESIAN_POINT('Origin',(-40.,-22.,10.));
#23653=CARTESIAN_POINT('',(-79.5,21.5,10.));
#23654=CARTESIAN_POINT('',(-42.9156148738428,21.5,10.));
#23655=CARTESIAN_POINT('',(-40.,21.5,10.));
#23656=CARTESIAN_POINT('',(-79.5,-21.5,10.));
#23657=CARTESIAN_POINT('',(-79.5,-11.,10.));
#23658=CARTESIAN_POINT('',(-42.9156148738428,-21.5,10.));
#23659=CARTESIAN_POINT('',(-40.,-21.5,10.));
#23660=CARTESIAN_POINT('',(-48.,-5.8783046359073E-15,10.));
#23661=CARTESIAN_POINT('Origin',(0.,0.,10.));
#23662=CARTESIAN_POINT('Origin',(0.,0.,10.));
#23663=CARTESIAN_POINT('',(-51.5,-1.5,10.));
#23664=CARTESIAN_POINT('',(-63.5,-1.5,10.));
#23665=CARTESIAN_POINT('',(-51.5,-1.5,10.));
#23666=CARTESIAN_POINT('',(-51.5,-17.5,10.));
#23667=CARTESIAN_POINT('',(-51.5,-12.,10.));
#23668=CARTESIAN_POINT('',(-63.5,-17.5,10.));
#23669=CARTESIAN_POINT('',(-46.,-17.5,10.));
#23670=CARTESIAN_POINT('',(-63.5,-19.5,10.));
#23671=CARTESIAN_POINT('',(-65.5,17.5,10.));
#23672=CARTESIAN_POINT('',(-77.5,17.5,10.));
#23673=CARTESIAN_POINT('',(-58.5,17.5,10.));
#23674=CARTESIAN_POINT('',(-65.5,1.5,10.));
#23675=CARTESIAN_POINT('',(-65.5,-2.5,10.));
#23676=CARTESIAN_POINT('',(-77.5,1.5,10.));
#23677=CARTESIAN_POINT('',(-53.,1.5,10.));
#23678=CARTESIAN_POINT('',(-77.5,-10.,10.));
#23679=CARTESIAN_POINT('',(-77.5,-17.5,10.));
#23680=CARTESIAN_POINT('',(-65.5,-17.5,10.));
#23681=CARTESIAN_POINT('',(-53.,-17.5,10.));
#23682=CARTESIAN_POINT('',(-77.5,-1.5,10.));
#23683=CARTESIAN_POINT('',(-77.5,-19.5,10.));
#23684=CARTESIAN_POINT('',(-65.5,-1.5,10.));
#23685=CARTESIAN_POINT('',(-58.5,-1.5,10.));
#23686=CARTESIAN_POINT('',(-65.5,-12.,10.));
#23687=CARTESIAN_POINT('Origin',(-65.75,-12.,9.75));
#23688=CARTESIAN_POINT('',(-66.,-2.,9.5));
#23689=CARTESIAN_POINT('',(-66.,-17.,9.5));
#23690=CARTESIAN_POINT('',(-66.,-12.,9.5));
#23691=CARTESIAN_POINT('',(-64.5,-18.5,11.));
#23692=CARTESIAN_POINT('',(-65.5,-1.5,10.));
#23693=CARTESIAN_POINT('Origin',(-58.5,-1.75,9.75));
#23694=CARTESIAN_POINT('',(-77.,-2.,9.5));
#23695=CARTESIAN_POINT('',(-58.5,-2.,9.5));
#23696=CARTESIAN_POINT('',(-77.5,-1.5,10.));
#23697=CARTESIAN_POINT('Origin',(-77.25,-19.5,9.75));
#23698=CARTESIAN_POINT('',(-77.,-17.,9.5));
#23699=CARTESIAN_POINT('',(-73.5833333333335,-13.5833333333334,6.08333333333338));
#23700=CARTESIAN_POINT('',(-77.,-19.5,9.5));
#23701=CARTESIAN_POINT('Origin',(-66.,-2.,10.));
#23702=CARTESIAN_POINT('',(-66.,-2.,4.));
#23703=CARTESIAN_POINT('',(-66.,-2.,10.));
#23704=CARTESIAN_POINT('',(-66.,-17.,4.));
#23705=CARTESIAN_POINT('',(-66.,-17.,4.));
#23706=CARTESIAN_POINT('',(-66.,-17.,10.));
#23707=CARTESIAN_POINT('Origin',(-77.,-2.,10.));
#23708=CARTESIAN_POINT('',(-77.,-2.,4.));
#23709=CARTESIAN_POINT('',(-77.,-2.,10.));
#23710=CARTESIAN_POINT('',(-66.,-2.,4.));
#23711=CARTESIAN_POINT('Origin',(-77.,-17.,10.));
#23712=CARTESIAN_POINT('',(-77.,-17.,4.));
#23713=CARTESIAN_POINT('',(-77.,-17.,10.));
#23714=CARTESIAN_POINT('',(-77.,-2.,4.));
#23715=CARTESIAN_POINT('Origin',(-77.25,-10.,9.75));
#23716=CARTESIAN_POINT('',(-77.,2.,9.5));
#23717=CARTESIAN_POINT('',(-75.1666666666668,3.83333333333328,7.66666666666671));
#23718=CARTESIAN_POINT('',(-77.,17.,9.5));
#23719=CARTESIAN_POINT('',(-77.,-10.,9.5));
#23720=CARTESIAN_POINT('',(-69.5833333333335,9.58333333333329,2.08333333333329));
#23721=CARTESIAN_POINT('Origin',(-77.,2.,10.));
#23722=CARTESIAN_POINT('',(-77.,2.,4.));
#23723=CARTESIAN_POINT('',(-77.,2.,10.));
#23724=CARTESIAN_POINT('',(-77.,17.,4.));
#23725=CARTESIAN_POINT('',(-77.,17.,4.));
#23726=CARTESIAN_POINT('',(-77.,17.,10.));
#23727=CARTESIAN_POINT('Origin',(-65.75,-2.5,9.75));
#23728=CARTESIAN_POINT('',(-66.,17.,9.5));
#23729=CARTESIAN_POINT('',(-67.8333333333333,15.1666666666667,7.66666666666666));
#23730=CARTESIAN_POINT('',(-66.,2.,9.5));
#23731=CARTESIAN_POINT('',(-66.,-2.5,9.5));
#23732=CARTESIAN_POINT('',(-62.9166666666667,-1.08333333333333,12.5833333333333));
#23733=CARTESIAN_POINT('Origin',(-66.,17.,10.));
#23734=CARTESIAN_POINT('',(-66.,17.,4.));
#23735=CARTESIAN_POINT('',(-66.,17.,10.));
#23736=CARTESIAN_POINT('',(-66.,2.,4.));
#23737=CARTESIAN_POINT('',(-66.,2.,4.));
#23738=CARTESIAN_POINT('',(-66.,2.,10.));
#23739=CARTESIAN_POINT('Origin',(-63.25,-19.5,9.75));
#23740=CARTESIAN_POINT('',(-63.,-17.,9.5));
#23741=CARTESIAN_POINT('',(-60.75,-14.75,7.24999999999999));
#23742=CARTESIAN_POINT('',(-63.,-2.,9.5));
#23743=CARTESIAN_POINT('',(-63.,-19.5,9.5));
#23744=CARTESIAN_POINT('',(-58.3333333333333,-6.66666666666663,4.83333333333335));
#23745=CARTESIAN_POINT('Origin',(-63.,-17.,10.));
#23746=CARTESIAN_POINT('',(-63.,-17.,4.));
#23747=CARTESIAN_POINT('',(-63.,-17.,10.));
#23748=CARTESIAN_POINT('',(-63.,-2.,4.));
#23749=CARTESIAN_POINT('',(-63.,-2.,4.));
#23750=CARTESIAN_POINT('',(-63.,-2.,10.));
#23751=CARTESIAN_POINT('Origin',(-51.75,-12.,9.75));
#23752=CARTESIAN_POINT('',(-52.,-2.,9.5));
#23753=CARTESIAN_POINT('',(-53.4166666666667,-3.41666666666665,8.08333333333335));
#23754=CARTESIAN_POINT('',(-52.,-17.,9.5));
#23755=CARTESIAN_POINT('',(-52.,-12.,9.5));
#23756=CARTESIAN_POINT('',(-51.6666666666667,-17.3333333333333,9.83333333333334));
#23757=CARTESIAN_POINT('Origin',(-52.,-2.,10.));
#23758=CARTESIAN_POINT('',(-52.,-2.,4.));
#23759=CARTESIAN_POINT('',(-52.,-2.,10.));
#23760=CARTESIAN_POINT('',(-52.,-17.,4.));
#23761=CARTESIAN_POINT('',(-52.,-17.,4.));
#23762=CARTESIAN_POINT('',(-52.,-17.,10.));
#23763=CARTESIAN_POINT('Origin',(-79.5,-21.5,10.));
#23764=CARTESIAN_POINT('',(-79.5,-21.75,9.56698729810778));
#23765=CARTESIAN_POINT('',(-80.,-21.1339745962156,9.5));
#23766=CARTESIAN_POINT('',(-79.5,-21.75,9.56698729810778));
#23767=CARTESIAN_POINT('',(-79.5,-21.5,10.));
#23768=CARTESIAN_POINT('',(-80.,-21.1339745962156,9.5));
#23769=CARTESIAN_POINT('Origin',(-40.,-21.625,9.78349364905389));
#23770=CARTESIAN_POINT('',(-42.7894554767877,-21.75,9.56698729810778));
#23771=CARTESIAN_POINT('Origin',(0.,0.,47.239092362731));
#23772=CARTESIAN_POINT('',(-40.,-21.75,9.56698729810778));
#23773=CARTESIAN_POINT('Origin',(-79.5,21.75,9.56698729810778));
#23774=CARTESIAN_POINT('',(-80.,21.1339745962156,9.5));
#23775=CARTESIAN_POINT('',(-79.5,21.5,10.));
#23776=CARTESIAN_POINT('',(-79.5,21.75,9.56698729810778));
#23777=CARTESIAN_POINT('',(-79.5,21.75,9.56698729810778));
#23778=CARTESIAN_POINT('',(-80.,21.1339745962156,9.5));
#23779=CARTESIAN_POINT('Origin',(-40.,21.625,9.78349364905389));
#23780=CARTESIAN_POINT('',(-42.7894554767877,21.75,9.56698729810778));
#23781=CARTESIAN_POINT('Origin',(0.,0.,47.239092362731));
#23782=CARTESIAN_POINT('',(-40.,21.75,9.56698729810778));
#23783=CARTESIAN_POINT('Origin',(-79.75,17.9509618943233,3.48686027918559));
#23784=CARTESIAN_POINT('',(-79.7165063509461,16.1014973081037,0.216506350946106));
#23785=CARTESIAN_POINT('',(-80.,15.9378221735089,0.5));
#23786=CARTESIAN_POINT('',(-82.202059880349,14.6664623088178,2.70205988034902));
#23787=CARTESIAN_POINT('',(-80.,17.7344555433772,3.61186027918559));
#23788=CARTESIAN_POINT('',(-79.5,16.4764973081037,0.433012701892218));
#23789=CARTESIAN_POINT('',(-79.5,18.1674682452695,3.36186027918558));
#23790=CARTESIAN_POINT('',(-73.1008330249197,27.5601796350596,6.83217967697247));
#23791=CARTESIAN_POINT('Origin',(-79.75,-11.,9.75));
#23792=CARTESIAN_POINT('',(-80.,-11.,9.5));
#23793=CARTESIAN_POINT('Origin',(-79.75,-15.0642105483752,-1.51313972081441));
#23794=CARTESIAN_POINT('',(-79.7165063509461,-16.1014973081037,0.216506350946103));
#23795=CARTESIAN_POINT('',(-79.5,-16.4764973081037,0.433012701892219));
#23796=CARTESIAN_POINT('',(-74.1008330249196,-25.8281288274908,5.83217967697252));
#23797=CARTESIAN_POINT('',(-79.5,-15.2807168993213,-1.63813972081441));
#23798=CARTESIAN_POINT('',(-80.,-15.9378221735089,0.5));
#23799=CARTESIAN_POINT('',(-80.,-14.8477041974291,-1.38813972081441));
#23800=CARTESIAN_POINT('',(-81.4877741660632,-15.078855358239,1.98777416606325));
#23801=CARTESIAN_POINT('Origin',(-40.,-16.2264973081037,1.11022302462516E-15));
#23802=CARTESIAN_POINT('',(-45.0122066014966,-16.4764973081037,0.433012701892212));
#23803=CARTESIAN_POINT('',(-20.,-16.4764973081037,0.433012701892219));
#23804=CARTESIAN_POINT('',(-45.069380727806,-16.5151724426986,0.500000000000003));
#23805=CARTESIAN_POINT('Ctrl Pts',(-45.0122066014946,-16.4764973081024,
0.433012701889958));
#23806=CARTESIAN_POINT('Ctrl Pts',(-45.0407770600794,-16.4958226019871,
0.466485092769431));
#23807=CARTESIAN_POINT('Ctrl Pts',(-45.0693807278045,-16.5151724426975,
0.499999999998238));
#23808=CARTESIAN_POINT('Origin',(0.,0.,-28.1051177665153));
#23809=CARTESIAN_POINT('Origin',(-20.,-16.1014973081037,0.216506350946109));
#23810=CARTESIAN_POINT('',(-79.5,-15.7264973081037,0.));
#23811=CARTESIAN_POINT('',(-70.9626933041054,-0.939448351016254,-8.53730669589464));
#23812=CARTESIAN_POINT('',(-44.8210584705248,-15.7264973081037,0.));
#23813=CARTESIAN_POINT('',(-10.,-15.7264973081037,-5.55111512312578E-16));
#23814=CARTESIAN_POINT('Origin',(8.88178419700125E-15,-33.2729580257087,
10.1304538186344));
#23815=CARTESIAN_POINT('Origin',(0.,0.,0.25));
#23816=CARTESIAN_POINT('',(3.3166247903554,47.3840690527945,0.));
#23817=CARTESIAN_POINT('',(3.9686269671671,47.8356561572586,0.500000000251442));
#23818=CARTESIAN_POINT('Ctrl Pts',(3.3166247903554,47.3840690527945,-2.4459601011273E-15));
#23819=CARTESIAN_POINT('Ctrl Pts',(3.46596392094177,47.4729188691332,0.0990603725345726));
#23820=CARTESIAN_POINT('Ctrl Pts',(3.60680863663856,47.5657711324945,0.202162724737091));
#23821=CARTESIAN_POINT('Ctrl Pts',(3.81688656552239,47.7171537854101,0.369509508930015));
#23822=CARTESIAN_POINT('Ctrl Pts',(3.89366123433624,47.7755348972366,0.433886438519603));
#23823=CARTESIAN_POINT('Ctrl Pts',(3.96862696690834,47.8356561575557,0.50000000027468));
#23824=CARTESIAN_POINT('Origin',(0.,0.,0.5));
#23825=CARTESIAN_POINT('Origin',(0.,0.,0.));
#23826=CARTESIAN_POINT('Origin',(0.,49.5,5.));
#23827=CARTESIAN_POINT('',(3.3166247903554,47.,0.));
#23828=CARTESIAN_POINT('',(3.3166247903554,49.5,0.));
#23829=CARTESIAN_POINT('',(3.96862696659689,47.5,0.5));
#23830=CARTESIAN_POINT('Origin',(0.,52.,5.));
#23831=CARTESIAN_POINT('',(-3.96862696659689,47.5,0.5));
#23832=CARTESIAN_POINT('Origin',(0.,47.5,5.));
#23833=CARTESIAN_POINT('',(-3.3166247903554,47.,0.));
#23834=CARTESIAN_POINT('Origin',(0.,52.,5.));
#23835=CARTESIAN_POINT('',(-3.3166247903554,47.3840690527945,0.));
#23836=CARTESIAN_POINT('',(-3.3166247903554,49.5,0.));
#23837=CARTESIAN_POINT('',(-3.9686269671671,47.8356561572586,0.500000000251442));
#23838=CARTESIAN_POINT('Ctrl Pts',(-3.96862696690834,47.8356561575557,0.500000000274678));
#23839=CARTESIAN_POINT('Ctrl Pts',(-3.89366123433624,47.7755348972366,0.4338864385196));
#23840=CARTESIAN_POINT('Ctrl Pts',(-3.8168865655224,47.7171537854101,0.369509508930017));
#23841=CARTESIAN_POINT('Ctrl Pts',(-3.60680863663856,47.5657711324945,0.202162724737091));
#23842=CARTESIAN_POINT('Ctrl Pts',(-3.46596392094177,47.4729188691332,0.0990603725345772));
#23843=CARTESIAN_POINT('Ctrl Pts',(-3.3166247903554,47.3840690527945,1.28369537222284E-15));
#23844=CARTESIAN_POINT('Ctrl Pts',(3.96862696704285,47.8356561572689,0.500000000393301));
#23845=CARTESIAN_POINT('Ctrl Pts',(4.0635320006758,47.8277824767126,0.583698372797031));
#23846=CARTESIAN_POINT('Ctrl Pts',(4.15494510797109,47.8199140758281,0.669663733732518));
#23847=CARTESIAN_POINT('Ctrl Pts',(4.77491092706035,47.7649010053097,1.28962955282178));
#23848=CARTESIAN_POINT('Ctrl Pts',(5.23654048654341,47.7145022029886,1.96378470873662));
#23849=CARTESIAN_POINT('Ctrl Pts',(5.84910641869338,47.6432894697029,3.44182385251829));
#23850=CARTESIAN_POINT('Ctrl Pts',(6.,47.6235235991626,4.24577588428941));
#23851=CARTESIAN_POINT('Ctrl Pts',(6.,47.6235235991626,5.));
#23852=CARTESIAN_POINT('Ctrl Pts',(6.,47.6235235991626,5.75422411571059));
#23853=CARTESIAN_POINT('Ctrl Pts',(5.84910641869338,47.6432894697029,6.55817614748171));
#23854=CARTESIAN_POINT('Ctrl Pts',(5.23654048654341,47.7145022029886,8.03621529126338));
#23855=CARTESIAN_POINT('Ctrl Pts',(4.77491092706036,47.7649010053097,8.71037044717822));
#23856=CARTESIAN_POINT('Ctrl Pts',(3.71037489380949,47.859363303171,9.77490648042908));
#23857=CARTESIAN_POINT('Ctrl Pts',(3.03621780475891,47.9095897499151,10.2365395235958));
#23858=CARTESIAN_POINT('Ctrl Pts',(1.55817211535174,47.980407545225,10.8491080110314));
#23859=CARTESIAN_POINT('Ctrl Pts',(0.754217814857577,48.,11.));
#23860=CARTESIAN_POINT('Ctrl Pts',(-0.754217814857576,48.,11.));
#23861=CARTESIAN_POINT('Ctrl Pts',(-1.55817211535174,47.980407545225,10.8491080110314));
#23862=CARTESIAN_POINT('Ctrl Pts',(-3.0362178047589,47.9095897499151,10.2365395235958));
#23863=CARTESIAN_POINT('Ctrl Pts',(-3.71037489380949,47.859363303171,9.77490648042908));
#23864=CARTESIAN_POINT('Ctrl Pts',(-4.77491092706036,47.7649010053097,8.71037044717822));
#23865=CARTESIAN_POINT('Ctrl Pts',(-5.23654048654341,47.7145022029886,8.03621529126338));
#23866=CARTESIAN_POINT('Ctrl Pts',(-5.84910641869338,47.6432894697029,6.55817614748171));
#23867=CARTESIAN_POINT('Ctrl Pts',(-6.,47.6235235991626,5.75422411571059));
#23868=CARTESIAN_POINT('Ctrl Pts',(-6.,47.6235235991626,4.24577588428941));
#23869=CARTESIAN_POINT('Ctrl Pts',(-5.84910641869338,47.6432894697029,3.44182385251829));
#23870=CARTESIAN_POINT('Ctrl Pts',(-5.23654048654342,47.7145022029886,1.96378470873662));
#23871=CARTESIAN_POINT('Ctrl Pts',(-4.77491092706036,47.7649010053097,1.28962955282179));
#23872=CARTESIAN_POINT('Ctrl Pts',(-4.15494510795552,47.8199140758295,0.66966373371695));
#23873=CARTESIAN_POINT('Ctrl Pts',(-4.06353200066262,47.8277824767137,0.583698372785401));
#23874=CARTESIAN_POINT('Ctrl Pts',(-3.96862696704285,47.8356561572689,0.500000000393302));
#23875=CARTESIAN_POINT('Origin',(0.,0.,0.));
#23876=CARTESIAN_POINT('',(-79.5,15.7264973081037,0.));
#23877=CARTESIAN_POINT('',(-79.5,0.,0.));
#23878=CARTESIAN_POINT('',(-44.8210584705248,15.7264973081037,0.));
#23879=CARTESIAN_POINT('',(-10.,15.7264973081037,0.));
#23880=CARTESIAN_POINT('Origin',(0.,0.,0.));
#23881=CARTESIAN_POINT('',(0.,47.,0.));
#23882=CARTESIAN_POINT('',(13.130339887499,11.7557050458495,0.));
#23883=CARTESIAN_POINT('Origin',(16.1803398874989,11.7557050458495,0.));
#23884=CARTESIAN_POINT('',(19.5,1.40834381901946E-15,0.));
#23885=CARTESIAN_POINT('Origin',(31.,0.,0.));
#23886=CARTESIAN_POINT('Origin',(0.,0.,0.25));
#23887=CARTESIAN_POINT('',(-45.0122066014966,16.4764973081037,0.43301270189222));
#23888=CARTESIAN_POINT('',(-45.069380727806,16.5151724426986,0.500000000000003));
#23889=CARTESIAN_POINT('Ctrl Pts',(-45.0693807278045,16.5151724426975,0.499999999998241));
#23890=CARTESIAN_POINT('Ctrl Pts',(-45.0407770600795,16.4958226019871,0.466485092769441));
#23891=CARTESIAN_POINT('Ctrl Pts',(-45.0122066014947,16.4764973081024,0.433012701889964));
#23892=CARTESIAN_POINT('Origin',(0.,0.,0.5));
#23893=CARTESIAN_POINT('Origin',(2.66453525910038E-14,33.2729580257085,
10.1304538186342));
#23894=CARTESIAN_POINT('Origin',(-53.,-17.25,9.75));
#23895=CARTESIAN_POINT('',(-53.,-17.,9.5));
#23896=CARTESIAN_POINT('Origin',(-66.,-17.,10.));
#23897=CARTESIAN_POINT('',(-77.,-17.,4.));
#23898=CARTESIAN_POINT('Origin',(-58.5,17.25,9.75));
#23899=CARTESIAN_POINT('',(-58.5,17.,9.5));
#23900=CARTESIAN_POINT('Origin',(-77.,17.,10.));
#23901=CARTESIAN_POINT('',(-66.,17.,4.));
#23902=CARTESIAN_POINT('Origin',(-53.,1.75,9.75));
#23903=CARTESIAN_POINT('',(-53.,2.,9.5));
#23904=CARTESIAN_POINT('Origin',(-66.,2.,10.));
#23905=CARTESIAN_POINT('',(-77.,2.,4.));
#23906=CARTESIAN_POINT('Origin',(-51.5,-1.75,9.75));
#23907=CARTESIAN_POINT('',(-51.5,-2.,9.5));
#23908=CARTESIAN_POINT('Origin',(-63.,-2.,10.));
#23909=CARTESIAN_POINT('',(-52.,-2.,4.));
#23910=CARTESIAN_POINT('Origin',(-46.,-17.25,9.75));
#23911=CARTESIAN_POINT('',(-46.,-17.,9.5));
#23912=CARTESIAN_POINT('Origin',(-52.,-17.,10.));
#23913=CARTESIAN_POINT('',(-63.,-17.,4.));
#23914=CARTESIAN_POINT('Origin',(16.1803398874989,11.7557050458495,0.25));
#23915=CARTESIAN_POINT('',(13.630339887499,11.7557050458495,0.5));
#23916=CARTESIAN_POINT('',(13.380339887499,11.7557050458495,0.25));
#23917=CARTESIAN_POINT('Origin',(16.1803398874989,11.7557050458495,0.5));
#23918=CARTESIAN_POINT('Origin',(16.1803398874989,11.7557050458495,0.));
#23919=CARTESIAN_POINT('',(13.630339887499,11.7557050458495,4.));
#23920=CARTESIAN_POINT('',(13.630339887499,11.7557050458495,0.));
#23921=CARTESIAN_POINT('Origin',(16.1803398874989,11.7557050458495,4.));
#23922=CARTESIAN_POINT('Origin',(-20.,16.1014973081037,0.216506350946109));
#23923=CARTESIAN_POINT('',(-20.,16.4764973081037,0.433012701892218));
#23924=CARTESIAN_POINT('',(-70.9626933041054,0.939448351016247,-8.5373066958946));
#23925=CARTESIAN_POINT('Origin',(-40.,22.,10.));
#23926=CARTESIAN_POINT('Origin',(0.,0.,-28.1051177665153));
#23927=CARTESIAN_POINT('Origin',(-79.75,0.,0.25));
#23928=CARTESIAN_POINT('',(-80.,0.,0.5));
#23929=CARTESIAN_POINT('Origin',(-80.,0.,5.));
#23930=CARTESIAN_POINT('Origin',(0.,47.25,0.25));
#23931=CARTESIAN_POINT('',(0.,47.5,0.5));
#23932=CARTESIAN_POINT('Origin',(0.,47.5,5.));
#23933=CARTESIAN_POINT('',(-2.55,47.5,5.));
#23934=CARTESIAN_POINT('Origin',(0.,47.5,5.));
#23935=CARTESIAN_POINT('Origin',(0.,-1.45875170827388E-15,13.1267766952966));
#23936=CARTESIAN_POINT('',(-47.6464466094067,-9.86076131526265E-31,13.5535533905933));
#23937=CARTESIAN_POINT('Origin',(0.,-2.91750341654776E-15,13.5535533905933));
#23938=CARTESIAN_POINT('',(-48.,-5.8783046359073E-15,12.7));
#23939=CARTESIAN_POINT('',(-47.8232233047034,-8.77415915104917E-15,13.1267766952966));
#23940=CARTESIAN_POINT('Origin',(0.,0.,12.7));
#23941=CARTESIAN_POINT('Origin',(0.,0.,13.6));
#23942=CARTESIAN_POINT('',(-47.5535533905933,-1.16472613895746E-14,13.6464466094067));
#23943=CARTESIAN_POINT('Origin',(0.,-2.91181534739364E-15,13.6464466094067));
#23944=CARTESIAN_POINT('',(-47.6,-5.8293187639414E-15,13.6));
#23945=CARTESIAN_POINT('Origin',(0.,0.,0.));
#23946=CARTESIAN_POINT('',(-48.,-5.8783046359073E-15,0.));
#23947=CARTESIAN_POINT('Origin',(31.,0.,0.25));
#23948=CARTESIAN_POINT('',(20.,-1.34711147906209E-15,0.5));
#23949=CARTESIAN_POINT('',(19.75,1.37772764904077E-15,0.25));
#23950=CARTESIAN_POINT('Origin',(31.,0.,0.5));
#23951=CARTESIAN_POINT('Origin',(31.,0.,14.));
#23952=CARTESIAN_POINT('',(20.,1.34711147906209E-15,13.4));
#23953=CARTESIAN_POINT('Origin',(31.,0.,13.4));
#23954=CARTESIAN_POINT('',(20.,1.34711147906209E-15,14.));
#23955=CARTESIAN_POINT('Origin',(0.,-1.45590767369682E-15,13.8232233047034));
#23956=CARTESIAN_POINT('',(-46.7,5.71910055201814E-15,14.));
#23957=CARTESIAN_POINT('',(-47.1267766952966,2.85955027600907E-15,13.8232233047034));
#23958=CARTESIAN_POINT('Origin',(0.,0.,14.));
#23959=CARTESIAN_POINT('Origin',(0.,0.,14.));
#23960=CARTESIAN_POINT('',(19.4,-1.42059028701093E-15,14.));
#23961=CARTESIAN_POINT('Origin',(31.,0.,14.));
#23962=CARTESIAN_POINT('',(-5.,-6.12323399573677E-16,14.));
#23963=CARTESIAN_POINT('Origin',(0.,0.,14.));
#23964=CARTESIAN_POINT('',(14.1303398874989,11.7557050458495,14.));
#23965=CARTESIAN_POINT('Origin',(16.1803398874989,11.7557050458495,14.));
#23966=CARTESIAN_POINT('Origin',(31.,0.,13.7));
#23967=CARTESIAN_POINT('',(19.7,-1.38385088303651E-15,13.7));
#23968=CARTESIAN_POINT('Origin',(0.,47.5,5.));
#23969=CARTESIAN_POINT('',(-2.55,35.5,5.));
#23970=CARTESIAN_POINT('',(-2.55,47.5,5.));
#23971=CARTESIAN_POINT('Origin',(0.,35.5,5.));
#23972=CARTESIAN_POINT('Origin',(0.,35.5,5.));
#23973=CARTESIAN_POINT('Origin',(16.1803398874989,11.7557050458495,4.));
#23974=CARTESIAN_POINT('',(14.1303398874989,11.7557050458495,4.));
#23975=CARTESIAN_POINT('Origin',(16.1803398874989,11.7557050458495,4.));
#23976=CARTESIAN_POINT('Origin',(16.1803398874989,11.7557050458495,14.));
#23977=CARTESIAN_POINT('',(14.1303398874989,11.7557050458495,14.));
#23978=CARTESIAN_POINT('Origin',(0.,0.,14.));
#23979=CARTESIAN_POINT('',(-5.,-6.12323399573677E-16,2.));
#23980=CARTESIAN_POINT('',(-5.,6.12323399573677E-16,14.));
#23981=CARTESIAN_POINT('Origin',(0.,0.,2.));
#23982=CARTESIAN_POINT('Origin',(0.,0.,2.));
#23983=CARTESIAN_POINT('Origin',(-57.5,-9.5,4.));
#23984=CARTESIAN_POINT('Origin',(-71.5,9.5,4.));
#23985=CARTESIAN_POINT('Origin',(-71.5,-9.5,4.));
#23986=CARTESIAN_POINT('Origin',(-52.,17.,10.));
#23987=CARTESIAN_POINT('',(-52.,17.,4.));
#23988=CARTESIAN_POINT('',(-52.,17.,10.));
#23989=CARTESIAN_POINT('',(-52.,2.,4.));
#23990=CARTESIAN_POINT('Origin',(-63.,17.,10.));
#23991=CARTESIAN_POINT('',(-52.,17.,4.));
#23992=CARTESIAN_POINT('Origin',(-57.5,9.5,4.));
#23993=CARTESIAN_POINT('',(0.,0.,0.));
#23994=CARTESIAN_POINT('Origin',(-2.67770341754863,53.2125144041213,14.5));
#23995=CARTESIAN_POINT('',(-2.29739178302164,53.0124970957195,11.0622545443402));
#23996=CARTESIAN_POINT('',(-3.0580150520755,53.412531712523,11.5));
#23997=CARTESIAN_POINT('Ctrl Pts',(-2.29739178302164,53.0124970957195,11.0622545443402));
#23998=CARTESIAN_POINT('Ctrl Pts',(-2.67614114120178,53.2116927560792,11.2776618075212));
#23999=CARTESIAN_POINT('Ctrl Pts',(-3.0580150520755,53.412531712523,11.5));
#24000=CARTESIAN_POINT('',(-3.0580150520755,53.412531712523,24.2));
#24001=CARTESIAN_POINT('',(-3.0580150520755,53.412531712523,14.5));
#24002=CARTESIAN_POINT('',(-2.29739178302176,53.0124970957196,24.2));
#24003=CARTESIAN_POINT('',(-2.43468625658982,53.0847043819776,24.2));
#24004=CARTESIAN_POINT('',(-2.29739178302176,53.0124970957196,14.5));
#24005=CARTESIAN_POINT('Origin',(0.,0.,14.5));
#24006=CARTESIAN_POINT('',(-4.4053330087579,53.318318063138,11.5));
#24007=CARTESIAN_POINT('Origin',(0.,0.,11.5));
#24008=CARTESIAN_POINT('',(-4.4053330087579,53.318318063138,24.2));
#24009=CARTESIAN_POINT('',(-4.4053330087579,53.318318063138,14.5));
#24010=CARTESIAN_POINT('Origin',(0.,0.,24.2));
#24011=CARTESIAN_POINT('Origin',(0.,0.,11.25));
#24012=CARTESIAN_POINT('',(-2.20794196160078,52.953989389792,11.));
#24013=CARTESIAN_POINT('Ctrl Pts',(-2.20794196160078,52.953989389792,11.));
#24014=CARTESIAN_POINT('Ctrl Pts',(-2.24054943696625,52.9719225189241,11.0192759649605));
#24015=CARTESIAN_POINT('Ctrl Pts',(-2.27052551750933,52.9918321844726,11.0404458048696));
#24016=CARTESIAN_POINT('Ctrl Pts',(-2.29739178302161,53.0124970957195,11.0622545443403));
#24017=CARTESIAN_POINT('',(-4.51126784227788,52.8076553394982,11.));
#24018=CARTESIAN_POINT('Origin',(0.,0.,11.));
#24019=CARTESIAN_POINT('',(-4.72678212511287,53.0869825079594,11.2969997378715));
#24020=CARTESIAN_POINT('Ctrl Pts',(-4.51126784227788,52.8076553394982,11.));
#24021=CARTESIAN_POINT('Ctrl Pts',(-4.57608660062692,52.8996682008571,11.0971961933879));
#24022=CARTESIAN_POINT('Ctrl Pts',(-4.64844098161557,52.9953004405385,11.1987310576086));
#24023=CARTESIAN_POINT('Ctrl Pts',(-4.72678212511288,53.0869825079594,11.2969997378715));
#24024=CARTESIAN_POINT('Ctrl Pts',(-4.4053330087579,53.318318063138,11.5));
#24025=CARTESIAN_POINT('Ctrl Pts',(-4.56636307296567,53.2024304236684,11.3977655520829));
#24026=CARTESIAN_POINT('Ctrl Pts',(-4.72678212511287,53.0869825079594,11.2969997378715));
#24027=CARTESIAN_POINT('Origin',(-46.653263217121,-25.7335348523128,14.5));
#24028=CARTESIAN_POINT('',(-46.6542861332861,-25.7671839061264,11.2969997378715));
#24029=CARTESIAN_POINT('',(-46.6663199357044,-26.1630385020257,11.5));
#24030=CARTESIAN_POINT('Ctrl Pts',(-46.6542861332861,-25.7671839061264,
11.2969997378715));
#24031=CARTESIAN_POINT('Ctrl Pts',(-46.6602915975399,-25.9647349828961,
11.3977655520833));
#24032=CARTESIAN_POINT('Ctrl Pts',(-46.6663199357044,-26.1630385020257,
11.5));
#24033=CARTESIAN_POINT('',(-46.6663199357044,-26.1630385020257,24.2));
#24034=CARTESIAN_POINT('',(-46.6663199357044,-26.1630385020257,14.5));
#24035=CARTESIAN_POINT('',(-46.6402064985376,-25.3040312025999,24.2));
#24036=CARTESIAN_POINT('',(-46.6449200416998,-25.459084248916,24.2));
#24037=CARTESIAN_POINT('',(-46.6402064985376,-25.3040312025999,11.5));
#24038=CARTESIAN_POINT('',(-46.6402064985376,-25.3040312025999,14.5));
#24039=CARTESIAN_POINT('Ctrl Pts',(-46.6402064985376,-25.3040312025999,
11.5));
#24040=CARTESIAN_POINT('Ctrl Pts',(-46.6463548096495,-25.5062812584034,
11.4654707447275));
#24041=CARTESIAN_POINT('Ctrl Pts',(-46.6542861332861,-25.7671839061264,
11.2969997378715));
#24042=CARTESIAN_POINT('Origin',(0.,0.,14.5));
#24043=CARTESIAN_POINT('',(-45.9910159507968,-27.3326993144394,11.5));
#24044=CARTESIAN_POINT('Origin',(0.,0.,11.5));
#24045=CARTESIAN_POINT('',(-45.9910159507968,-27.3326993144394,24.2));
#24046=CARTESIAN_POINT('',(-45.9910159507968,-27.3326993144394,14.5));
#24047=CARTESIAN_POINT('Origin',(0.,0.,24.2));
#24048=CARTESIAN_POINT('Origin',(0.,0.,11.25));
#24049=CARTESIAN_POINT('',(-46.3021993580384,-25.7896555736688,11.));
#24050=CARTESIAN_POINT('Ctrl Pts',(-46.6542861332861,-25.7671839061264,
11.2969997378715));
#24051=CARTESIAN_POINT('Ctrl Pts',(-46.5344704431712,-25.7808636960853,
11.1987310576086));
#24052=CARTESIAN_POINT('Ctrl Pts',(-46.4147276669438,-25.787371326691,11.0971961933879));
#24053=CARTESIAN_POINT('Ctrl Pts',(-46.3021993580384,-25.7896555736688,
11.));
#24054=CARTESIAN_POINT('',(-45.135512297021,-27.781028233049,11.));
#24055=CARTESIAN_POINT('Origin',(0.,0.,11.));
#24056=CARTESIAN_POINT('',(-45.2340370888743,-27.7395880641857,11.0622545443403));
#24057=CARTESIAN_POINT('Ctrl Pts',(-45.2340370888743,-27.7395880641857,
11.0622545443404));
#24058=CARTESIAN_POINT('Ctrl Pts',(-45.2018816759998,-27.7503055360096,
11.0404458048696));
#24059=CARTESIAN_POINT('Ctrl Pts',(-45.1686134036895,-27.7640234893725,
11.0192759649605));
#24060=CARTESIAN_POINT('Ctrl Pts',(-45.135512297021,-27.781028233049,11.));
#24061=CARTESIAN_POINT('Ctrl Pts',(-45.9910159507968,-27.3326993144394,
11.5));
#24062=CARTESIAN_POINT('Ctrl Pts',(-45.6109717288891,-27.5369794153495,
11.2776618075202));
#24063=CARTESIAN_POINT('Ctrl Pts',(-45.2340370888743,-27.7395880641857,
11.0622545443403));
#24064=CARTESIAN_POINT('Origin',(-45.6125265198356,-27.5361436893125,14.5));
#24065=CARTESIAN_POINT('',(-45.2340370888744,-27.7395880641857,24.2));
#24066=CARTESIAN_POINT('',(-45.3706737374995,-27.6661435891479,24.2));
#24067=CARTESIAN_POINT('',(-45.2340370888744,-27.7395880641857,14.5));
#24068=CARTESIAN_POINT('Origin',(-45.4553779539844,-28.4036725628998,11.));
#24069=CARTESIAN_POINT('',(-44.7555290624911,-28.3891285237239,11.));
#24070=CARTESIAN_POINT('Origin',(-45.4553779539844,-28.4036725628998,11.));
#24071=CARTESIAN_POINT('',(-44.7614733114311,-28.4958481944022,11.0622545443403));
#24072=CARTESIAN_POINT('Ctrl Pts',(-44.7555290624911,-28.3891285237239,
11.));
#24073=CARTESIAN_POINT('Ctrl Pts',(-44.7547558702061,-28.4263339903097,
11.0192759649605));
#24074=CARTESIAN_POINT('Ctrl Pts',(-44.7570101060804,-28.4622488703402,
11.0404458048696));
#24075=CARTESIAN_POINT('Ctrl Pts',(-44.7614733114311,-28.4958481944021,
11.0622545443403));
#24076=CARTESIAN_POINT('',(-44.7614733114311,-28.4958481944023,24.2));
#24077=CARTESIAN_POINT('',(-44.7614733114311,-28.4958481944023,14.5));
#24078=CARTESIAN_POINT('Origin',(-45.4553779539844,-28.4036725628998,24.2));
#24079=CARTESIAN_POINT('Origin',(-48.3346988609778,-22.4164821240926,14.5));
#24080=CARTESIAN_POINT('',(-48.3380665247094,-22.4499778554777,11.2969997378715));
#24081=CARTESIAN_POINT('',(-48.3776844341152,-22.8440287338545,11.5));
#24082=CARTESIAN_POINT('Ctrl Pts',(-48.3380665247094,-22.4499778554777,
11.2969997378715));
#24083=CARTESIAN_POINT('Ctrl Pts',(-48.3578378264537,-22.6466287877421,
11.3977655520825));
#24084=CARTESIAN_POINT('Ctrl Pts',(-48.3776844341152,-22.8440287338545,
11.5));
#24085=CARTESIAN_POINT('',(-48.3776844341152,-22.8440287338545,24.2));
#24086=CARTESIAN_POINT('',(-48.3776844341152,-22.8440287338545,14.5));
#24087=CARTESIAN_POINT('',(-48.2917132878405,-21.9889355143307,24.2));
#24088=CARTESIAN_POINT('',(-48.3072313028027,-22.1432820590691,24.2));
#24089=CARTESIAN_POINT('',(-48.2917132878405,-21.9889355143307,11.5));
#24090=CARTESIAN_POINT('',(-48.2917132878405,-21.9889355143307,14.5));
#24091=CARTESIAN_POINT('Ctrl Pts',(-48.2917132878405,-21.9889355143307,
11.5));
#24092=CARTESIAN_POINT('Ctrl Pts',(-48.3119548726829,-22.1902640146607,
11.4654707447276));
#24093=CARTESIAN_POINT('Ctrl Pts',(-48.3380665247094,-22.4499778554777,
11.2969997378715));
#24094=CARTESIAN_POINT('Origin',(-48.9660365296434,-21.8010840688629,11.25));
#24095=CARTESIAN_POINT('',(-48.6544270396318,-21.1742670894066,11.5));
#24096=CARTESIAN_POINT('Origin',(-48.9660365296434,-21.8010840688629,11.5));
#24097=CARTESIAN_POINT('',(-49.028064639274,-20.9002167162411,11.2969997378715));
#24098=CARTESIAN_POINT('Ctrl Pts',(-49.028064639274,-20.9002167162411,11.2969997378715));
#24099=CARTESIAN_POINT('Ctrl Pts',(-48.8175875368124,-21.0545944569385,
11.4654707447276));
#24100=CARTESIAN_POINT('Ctrl Pts',(-48.6544270396318,-21.1742670894066,
11.5));
#24101=CARTESIAN_POINT('',(-48.8290062914572,-20.608933611151,11.));
#24102=CARTESIAN_POINT('Ctrl Pts',(-49.028064639274,-20.9002167162411,11.2969997378715));
#24103=CARTESIAN_POINT('Ctrl Pts',(-48.9650785563254,-20.7973785443114,
11.1987310576086));
#24104=CARTESIAN_POINT('Ctrl Pts',(-48.8964856249514,-20.699013451518,11.0971961933879));
#24105=CARTESIAN_POINT('Ctrl Pts',(-48.8290062914572,-20.608933611151,11.));
#24106=CARTESIAN_POINT('',(-47.9884049594373,-22.4969551150606,11.));
#24107=CARTESIAN_POINT('Origin',(-48.9660365296434,-21.8010840688629,11.));
#24108=CARTESIAN_POINT('Ctrl Pts',(-48.3380665247094,-22.4499778554777,
11.2969997378715));
#24109=CARTESIAN_POINT('Ctrl Pts',(-48.2194969535028,-22.4719822421975,
11.1987310576086));
#24110=CARTESIAN_POINT('Ctrl Pts',(-48.1004998140235,-22.4868268543681,
11.0971961933879));
#24111=CARTESIAN_POINT('Ctrl Pts',(-47.9884049594373,-22.4969551150606,
11.));
#24112=CARTESIAN_POINT('Origin',(-48.9660365296434,-21.8010840688629,11.));
#24113=CARTESIAN_POINT('',(-48.6544270396318,-21.1742670894066,24.2));
#24114=CARTESIAN_POINT('Origin',(-48.9660365296434,-21.8010840688629,24.2));
#24115=CARTESIAN_POINT('',(-48.6544270396318,-21.1742670894066,14.5));
#24116=CARTESIAN_POINT('Origin',(-47.4222409819887,-24.2872980186631,14.5));
#24117=CARTESIAN_POINT('',(-47.7856168695246,-24.0579471360089,24.2));
#24118=CARTESIAN_POINT('',(-47.0588650944528,-24.5166489013173,24.2));
#24119=CARTESIAN_POINT('',(-47.1900456754746,-24.4338520425372,24.2));
#24120=CARTESIAN_POINT('',(-47.7856168695246,-24.0579471360089,11.5));
#24121=CARTESIAN_POINT('',(-47.7856168695246,-24.0579471360089,14.5));
#24122=CARTESIAN_POINT('',(-47.4507093193417,-24.2693297424964,11.2969997378715));
#24123=CARTESIAN_POINT('Ctrl Pts',(-47.7856168695246,-24.0579471360089,
11.5));
#24124=CARTESIAN_POINT('Ctrl Pts',(-47.6178447974743,-24.1638393378014,
11.3977655520829));
#24125=CARTESIAN_POINT('Ctrl Pts',(-47.4507093193417,-24.2693297424964,
11.2969997378715));
#24126=CARTESIAN_POINT('',(-47.0588650944528,-24.5166489013173,11.5));
#24127=CARTESIAN_POINT('Ctrl Pts',(-47.4507093193417,-24.2693297424964,
11.2969997378715));
#24128=CARTESIAN_POINT('Ctrl Pts',(-47.2299760817075,-24.4086492863049,
11.4654707447276));
#24129=CARTESIAN_POINT('Ctrl Pts',(-47.0588650944528,-24.5166489013173,
11.5));
#24130=CARTESIAN_POINT('',(-47.0588650944528,-24.5166489013173,14.5));
#24131=CARTESIAN_POINT('Origin',(-47.3259909772385,-25.1636757653237,11.));
#24132=CARTESIAN_POINT('Origin',(-47.3259909772385,-25.1636757653237,24.2));
#24133=CARTESIAN_POINT('Origin',(-47.3259909772385,-25.1636757653237,11.5));
#24134=CARTESIAN_POINT('Origin',(-47.3259909772385,-25.1636757653237,11.25));
#24135=CARTESIAN_POINT('',(-47.2724547499278,-23.9648705799974,11.));
#24136=CARTESIAN_POINT('Ctrl Pts',(-47.4507093193417,-24.2693297424964,
11.2969997378715));
#24137=CARTESIAN_POINT('Ctrl Pts',(-47.3950502955656,-24.1623483921435,
11.1987310576087));
#24138=CARTESIAN_POINT('Ctrl Pts',(-47.3334860551377,-24.0594381107558,
11.0971961933879));
#24139=CARTESIAN_POINT('Ctrl Pts',(-47.2724547499278,-23.9648705799974,
11.));
#24140=CARTESIAN_POINT('Origin',(-47.3259909772385,-25.1636757653237,11.));
#24141=CARTESIAN_POINT('Origin',(-49.7806527105708,-18.9902185482608,14.5));
#24142=CARTESIAN_POINT('',(-49.7863487149497,-19.0233977693811,11.2969997378715));
#24143=CARTESIAN_POINT('',(-49.8533577168707,-19.4137251539658,11.5));
#24144=CARTESIAN_POINT('Ctrl Pts',(-49.7863487149497,-19.0233977693811,
11.2969997378715));
#24145=CARTESIAN_POINT('Ctrl Pts',(-49.8197895303902,-19.2181904935679,
11.3977655520829));
#24146=CARTESIAN_POINT('Ctrl Pts',(-49.8533577168707,-19.4137251539658,
11.5));
#24147=CARTESIAN_POINT('',(-49.8533577168707,-19.4137251539658,24.2));
#24148=CARTESIAN_POINT('',(-49.8533577168707,-19.4137251539658,14.5));
#24149=CARTESIAN_POINT('',(-49.707947704271,-18.5667119425558,24.2));
#24150=CARTESIAN_POINT('',(-49.7341945888243,-18.7196000248653,24.2));
#24151=CARTESIAN_POINT('',(-49.707947704271,-18.5667119425558,11.5));
#24152=CARTESIAN_POINT('',(-49.707947704271,-18.5667119425558,14.5));
#24153=CARTESIAN_POINT('Ctrl Pts',(-49.707947704271,-18.5667119425558,11.5));
#24154=CARTESIAN_POINT('Ctrl Pts',(-49.7421839478772,-18.7661380351961,
11.4654707447276));
#24155=CARTESIAN_POINT('Ctrl Pts',(-49.7863487149497,-19.0233977693811,
11.2969997378715));
#24156=CARTESIAN_POINT('Origin',(-50.3675244741247,-18.3322796822558,11.25));
#24157=CARTESIAN_POINT('',(-50.0129495069995,-17.7287263766662,11.5));
#24158=CARTESIAN_POINT('Origin',(-50.3675244741247,-18.3322796822558,11.5));
#24159=CARTESIAN_POINT('',(-50.3665601565676,-17.4292799350267,11.2969997378715));
#24160=CARTESIAN_POINT('Ctrl Pts',(-50.3665601565676,-17.4292799350267,
11.2969997378715));
#24161=CARTESIAN_POINT('Ctrl Pts',(-50.1673646125647,-17.5979637597785,
11.4654707447276));
#24162=CARTESIAN_POINT('Ctrl Pts',(-50.0129495069995,-17.7287263766662,
11.5));
#24163=CARTESIAN_POINT('',(-50.1476678226092,-17.1525919893539,11.));
#24164=CARTESIAN_POINT('Ctrl Pts',(-50.3665601565676,-17.4292799350267,
11.2969997378715));
#24165=CARTESIAN_POINT('Ctrl Pts',(-50.2965538763113,-17.3310859587567,
11.1987310576086));
#24166=CARTESIAN_POINT('Ctrl Pts',(-50.221266431858,-17.237745279402,11.0971961933879));
#24167=CARTESIAN_POINT('Ctrl Pts',(-50.1476678226092,-17.1525919893539,
11.));
#24168=CARTESIAN_POINT('',(-49.4408158756514,-19.0946517525179,11.));
#24169=CARTESIAN_POINT('Origin',(-50.3675244741247,-18.3322796822558,11.));
#24170=CARTESIAN_POINT('Ctrl Pts',(-49.7863487149497,-19.0233977693811,
11.2969997378715));
#24171=CARTESIAN_POINT('Ctrl Pts',(-49.6696029216838,-19.0536195497014,
11.1987310576086));
#24172=CARTESIAN_POINT('Ctrl Pts',(-49.5519311610546,-19.0767288219785,
11.0971961933879));
#24173=CARTESIAN_POINT('Ctrl Pts',(-49.4408158756514,-19.0946517525179,
11.));
#24174=CARTESIAN_POINT('Origin',(-50.3675244741247,-18.3322796822558,11.));
#24175=CARTESIAN_POINT('',(-50.0129495069995,-17.7287263766662,24.2));
#24176=CARTESIAN_POINT('Origin',(-50.3675244741247,-18.3322796822558,24.2));
#24177=CARTESIAN_POINT('',(-50.0129495069995,-17.7287263766662,14.5));
#24178=CARTESIAN_POINT('Origin',(-49.0009190529448,-20.9201270734172,14.5));
#24179=CARTESIAN_POINT('',(-49.3474110662579,-20.6659870574277,24.2));
#24180=CARTESIAN_POINT('',(-48.7795124544456,-21.0825212248573,24.2));
#24181=CARTESIAN_POINT('',(-49.3474110662579,-20.6659870574277,11.5));
#24182=CARTESIAN_POINT('',(-49.3474110662579,-20.6659870574277,14.5));
#24183=CARTESIAN_POINT('Ctrl Pts',(-49.3474110662579,-20.6659870574277,
11.5));
#24184=CARTESIAN_POINT('Ctrl Pts',(-49.1874343451363,-20.7833244992782,
11.3977655520826));
#24185=CARTESIAN_POINT('Ctrl Pts',(-49.028064639274,-20.9002167162411,11.2969997378715));
#24186=CARTESIAN_POINT('Origin',(-50.34086957183,-17.4510353719535,14.5));
#24187=CARTESIAN_POINT('',(-50.6687896366606,-17.1733443672407,24.2));
#24188=CARTESIAN_POINT('',(-50.131330352038,-17.6284784829776,24.2));
#24189=CARTESIAN_POINT('',(-50.6687896366606,-17.1733443672407,11.5));
#24190=CARTESIAN_POINT('',(-50.6687896366606,-17.1733443672407,14.5));
#24191=CARTESIAN_POINT('Ctrl Pts',(-50.6687896366606,-17.1733443672407,
11.5));
#24192=CARTESIAN_POINT('Ctrl Pts',(-50.5173876569737,-17.3015553929261,
11.3977655520831));
#24193=CARTESIAN_POINT('Ctrl Pts',(-50.3665601565676,-17.4292799350267,
11.2969997378715));
#24194=CARTESIAN_POINT('Origin',(-52.6411144591754,8.22525703532524,14.5));
#24195=CARTESIAN_POINT('',(-52.8002826611136,8.62439278479967,24.2));
#24196=CARTESIAN_POINT('',(-52.4819462572371,7.8261212858508,24.2));
#24197=CARTESIAN_POINT('',(-52.5394068040886,7.97021136259658,24.2));
#24198=CARTESIAN_POINT('',(-52.8002826611136,8.62439278479967,11.5));
#24199=CARTESIAN_POINT('',(-52.8002826611136,8.62439278479967,14.5));
#24200=CARTESIAN_POINT('',(-52.4819462572371,7.82612128585067,11.0622545443402));
#24201=CARTESIAN_POINT('Ctrl Pts',(-52.8002826611136,8.62439278479967,11.5));
#24202=CARTESIAN_POINT('Ctrl Pts',(-52.6404606145519,8.22361743168168,11.2776618075197));
#24203=CARTESIAN_POINT('Ctrl Pts',(-52.4819462572371,7.82612128585067,11.0622545443402));
#24204=CARTESIAN_POINT('',(-52.4819462572371,7.8261212858508,14.5));
#24205=CARTESIAN_POINT('Origin',(-53.0783684845482,7.4596782114595,11.));
#24206=CARTESIAN_POINT('',(-52.4331091150171,7.73104575932093,11.));
#24207=CARTESIAN_POINT('Ctrl Pts',(-52.481946257237,7.82612128585063,11.0622545443403));
#24208=CARTESIAN_POINT('Ctrl Pts',(-52.4642028399839,7.79724212513569,11.0404458048696));
#24209=CARTESIAN_POINT('Ctrl Pts',(-52.4475355953004,7.76534912995433,11.0192759649605));
#24210=CARTESIAN_POINT('Ctrl Pts',(-52.4331091150171,7.73104575932093,11.));
#24211=CARTESIAN_POINT('',(-52.5329044020197,7.0209653957459,11.));
#24212=CARTESIAN_POINT('Origin',(-53.0783684845482,7.4596782114595,11.));
#24213=CARTESIAN_POINT('',(-52.6060560429105,6.94303427461877,11.0622545443404));
#24214=CARTESIAN_POINT('Ctrl Pts',(-52.6060560429105,6.94303427461877,11.0622545443404));
#24215=CARTESIAN_POINT('Ctrl Pts',(-52.5810436316806,6.96590045416114,11.0404491452186));
#24216=CARTESIAN_POINT('Ctrl Pts',(-52.5562282907997,6.99196614352735,11.0192767711931));
#24217=CARTESIAN_POINT('Ctrl Pts',(-52.5329044020197,7.02096539574591,11.));
#24218=CARTESIAN_POINT('',(-52.6060560429105,6.94303427461877,24.2));
#24219=CARTESIAN_POINT('',(-52.6060560429105,6.94303427461877,14.5));
#24220=CARTESIAN_POINT('Origin',(-53.0783684845482,7.4596782114595,24.2));
#24221=CARTESIAN_POINT('Origin',(0.,0.,11.25));
#24222=CARTESIAN_POINT('',(-52.5657520484127,9.95448198475441,11.5));
#24223=CARTESIAN_POINT('Origin',(0.,0.,11.5));
#24224=CARTESIAN_POINT('',(-51.9935887462791,10.5957343592208,11.0622545443404));
#24225=CARTESIAN_POINT('Ctrl Pts',(-52.5657520484127,9.95448198475441,11.5));
#24226=CARTESIAN_POINT('Ctrl Pts',(-52.3754957821832,10.1677118127105,11.3527407245743));
#24227=CARTESIAN_POINT('Ctrl Pts',(-52.184766529217,10.3814717408442,11.2067970124645));
#24228=CARTESIAN_POINT('Ctrl Pts',(-51.9935887462791,10.5957343592208,11.0622545443404));
#24229=CARTESIAN_POINT('',(-51.9151790989041,10.6683728435365,11.));
#24230=CARTESIAN_POINT('Ctrl Pts',(-51.9935887462791,10.5957343592208,11.0622545443404));
#24231=CARTESIAN_POINT('Ctrl Pts',(-51.9670422000274,10.6168000602485,11.0404491452634));
#24232=CARTESIAN_POINT('Ctrl Pts',(-51.940469057341,10.6410712243803,11.0192767711182));
#24233=CARTESIAN_POINT('Ctrl Pts',(-51.9151790989041,10.6683728435365,11.));
#24234=CARTESIAN_POINT('Origin',(0.,0.,11.));
#24235=CARTESIAN_POINT('Origin',(-51.4355644344077,13.8969239803297,14.5));
#24236=CARTESIAN_POINT('',(-51.4596748556074,13.8734294539541,11.2969997378715));
#24237=CARTESIAN_POINT('',(-51.7433149571623,13.5970348695554,11.5));
#24238=CARTESIAN_POINT('Ctrl Pts',(-51.4596748556074,13.8734294539541,11.2969997378715));
#24239=CARTESIAN_POINT('Ctrl Pts',(-51.6012253341346,13.7354948478477,11.3977655520825));
#24240=CARTESIAN_POINT('Ctrl Pts',(-51.7433149571623,13.5970348695554,11.5));
#24241=CARTESIAN_POINT('',(-51.7433149571623,13.5970348695554,24.2));
#24242=CARTESIAN_POINT('',(-51.7433149571623,13.5970348695554,14.5));
#24243=CARTESIAN_POINT('',(-51.1278139116531,14.1968130911041,24.2));
#24244=CARTESIAN_POINT('',(-51.238913447339,14.0885515659373,24.2));
#24245=CARTESIAN_POINT('',(-51.1278139116531,14.1968130911041,11.5));
#24246=CARTESIAN_POINT('',(-51.1278139116531,14.1968130911041,14.5));
#24247=CARTESIAN_POINT('Ctrl Pts',(-51.1278139116531,14.1968130911041,11.5));
#24248=CARTESIAN_POINT('Ctrl Pts',(-51.2727313307305,14.055597552122,11.4654707447276));
#24249=CARTESIAN_POINT('Ctrl Pts',(-51.4596748556074,13.8734294539541,11.2969997378715));
#24250=CARTESIAN_POINT('Origin',(0.,0.,14.5));
#24251=CARTESIAN_POINT('',(-52.0700565974321,12.286545728569,11.5));
#24252=CARTESIAN_POINT('Origin',(0.,0.,11.5));
#24253=CARTESIAN_POINT('',(-52.0700565974321,12.286545728569,24.2));
#24254=CARTESIAN_POINT('',(-52.0700565974321,12.286545728569,14.5));
#24255=CARTESIAN_POINT('Origin',(0.,0.,24.2));
#24256=CARTESIAN_POINT('Origin',(0.,0.,11.25));
#24257=CARTESIAN_POINT('',(-51.2220149569553,13.6126846635571,11.));
#24258=CARTESIAN_POINT('Ctrl Pts',(-51.4596748556074,13.8734294539541,11.2969997378715));
#24259=CARTESIAN_POINT('Ctrl Pts',(-51.3829894416038,13.7803580645257,11.1987310576087));
#24260=CARTESIAN_POINT('Ctrl Pts',(-51.3013742769325,13.6924965450168,11.0971961933879));
#24261=CARTESIAN_POINT('Ctrl Pts',(-51.2220149569553,13.6126846635571,11.));
#24262=CARTESIAN_POINT('',(-51.766094205967,11.3697621197168,11.));
#24263=CARTESIAN_POINT('Origin',(0.,0.,11.));
#24264=CARTESIAN_POINT('',(-51.8081802498931,11.4680127538716,11.0622545443405));
#24265=CARTESIAN_POINT('Ctrl Pts',(-51.766094205967,11.3697621197168,11.));
#24266=CARTESIAN_POINT('Ctrl Pts',(-51.7780925319007,11.4049878878031,11.0192757561174));
#24267=CARTESIAN_POINT('Ctrl Pts',(-51.7924947217674,11.4379665269991,11.0404460254343));
#24268=CARTESIAN_POINT('Ctrl Pts',(-51.8081802498931,11.4680127538716,11.0622545443405));
#24269=CARTESIAN_POINT('Ctrl Pts',(-52.0700565974321,12.286545728569,11.5));
#24270=CARTESIAN_POINT('Ctrl Pts',(-51.9829772340571,12.0143663927566,11.352740724575));
#24271=CARTESIAN_POINT('Ctrl Pts',(-51.8956813869632,11.7415104052956,11.2067970124648));
#24272=CARTESIAN_POINT('Ctrl Pts',(-51.8081802498931,11.4680127538716,11.0622545443405));
#24273=CARTESIAN_POINT('Origin',(-50.9840802240917,15.4714365365517,14.5));
#24274=CARTESIAN_POINT('',(-51.0861504520718,15.8888398565875,24.2));
#24275=CARTESIAN_POINT('',(-50.8820099961117,15.054033216516,24.2));
#24276=CARTESIAN_POINT('',(-50.9188578780728,15.204717981028,24.2));
#24277=CARTESIAN_POINT('',(-51.0861504520718,15.8888398565875,11.5));
#24278=CARTESIAN_POINT('',(-51.0861504520718,15.8888398565875,14.5));
#24279=CARTESIAN_POINT('',(-50.9920768187572,15.5041376015772,11.2969997378715));
#24280=CARTESIAN_POINT('Ctrl Pts',(-51.0861504520718,15.8888398565875,11.5));
#24281=CARTESIAN_POINT('Ctrl Pts',(-51.0390242276022,15.6961231071135,11.3977655520829));
#24282=CARTESIAN_POINT('Ctrl Pts',(-50.9920768187572,15.5041376015772,11.2969997378715));
#24283=CARTESIAN_POINT('',(-50.8820099961117,15.054033216516,11.5));
#24284=CARTESIAN_POINT('Ctrl Pts',(-50.9920768187572,15.5041376015772,11.2969997378715));
#24285=CARTESIAN_POINT('Ctrl Pts',(-50.9300741029444,15.2505853175896,11.4654707447276));
#24286=CARTESIAN_POINT('Ctrl Pts',(-50.8820099961117,15.054033216516,11.5));
#24287=CARTESIAN_POINT('',(-50.8820099961117,15.054033216516,14.5));
#24288=CARTESIAN_POINT('Origin',(0.,0.,11.25));
#24289=CARTESIAN_POINT('',(-50.6687896366605,17.173344367241,11.5));
#24290=CARTESIAN_POINT('Origin',(0.,0.,11.5));
#24291=CARTESIAN_POINT('',(-50.3665601565677,17.4292799350268,11.2969997378715));
#24292=CARTESIAN_POINT('Ctrl Pts',(-50.3665601565677,17.4292799350268,11.2969997378715));
#24293=CARTESIAN_POINT('Ctrl Pts',(-50.5173876569729,17.301555392927,11.3977655520826));
#24294=CARTESIAN_POINT('Ctrl Pts',(-50.6687896366605,17.173344367241,11.5));
#24295=CARTESIAN_POINT('',(-50.1476678226092,17.1525919893539,11.));
#24296=CARTESIAN_POINT('Ctrl Pts',(-50.3665601565677,17.4292799350268,11.2969997378715));
#24297=CARTESIAN_POINT('Ctrl Pts',(-50.2965538763113,17.3310859587568,11.1987310576087));
#24298=CARTESIAN_POINT('Ctrl Pts',(-50.221266431858,17.237745279402,11.0971961933879));
#24299=CARTESIAN_POINT('Ctrl Pts',(-50.1476678226092,17.1525919893539,11.));
#24300=CARTESIAN_POINT('',(-50.6523561066928,15.5993211660246,11.));
#24301=CARTESIAN_POINT('Origin',(0.,0.,11.));
#24302=CARTESIAN_POINT('Ctrl Pts',(-50.9920768187572,15.5041376015772,11.2969997378715));
#24303=CARTESIAN_POINT('Ctrl Pts',(-50.8777235772014,15.5424295380224,11.1987310576087));
#24304=CARTESIAN_POINT('Ctrl Pts',(-50.7619504804118,15.5736908843544,11.0971961933879));
#24305=CARTESIAN_POINT('Ctrl Pts',(-50.6523561066928,15.5993211660246,11.));
#24306=CARTESIAN_POINT('Origin',(0.,0.,14.5));
#24307=CARTESIAN_POINT('',(-50.6687896366605,17.173344367241,24.2));
#24308=CARTESIAN_POINT('Origin',(0.,0.,24.2));
#24309=CARTESIAN_POINT('',(-50.6687896366605,17.173344367241,14.5));
#24310=CARTESIAN_POINT('Origin',(-50.3408695718299,17.4510353719536,14.5));
#24311=CARTESIAN_POINT('',(-50.0129495069994,17.7287263766663,24.2));
#24312=CARTESIAN_POINT('',(-50.131330352038,17.6284784829776,24.2));
#24313=CARTESIAN_POINT('',(-50.0129495069994,17.7287263766663,11.5));
#24314=CARTESIAN_POINT('',(-50.0129495069994,17.7287263766663,14.5));
#24315=CARTESIAN_POINT('Ctrl Pts',(-50.0129495069994,17.7287263766663,11.5));
#24316=CARTESIAN_POINT('Ctrl Pts',(-50.1673646125647,17.5979637597785,11.4654707447276));
#24317=CARTESIAN_POINT('Ctrl Pts',(-50.3665601565677,17.4292799350268,11.2969997378715));
#24318=CARTESIAN_POINT('Origin',(-49.7806527105709,18.9902185482606,14.5));
#24319=CARTESIAN_POINT('',(-49.8533577168709,19.4137251539655,24.2));
#24320=CARTESIAN_POINT('',(-49.7079477042709,18.5667119425557,24.2));
#24321=CARTESIAN_POINT('',(-49.7341945888243,18.7196000248653,24.2));
#24322=CARTESIAN_POINT('',(-49.8533577168709,19.4137251539655,11.5));
#24323=CARTESIAN_POINT('',(-49.8533577168709,19.4137251539655,14.5));
#24324=CARTESIAN_POINT('',(-49.7863487149498,19.0233977693811,11.2969997378715));
#24325=CARTESIAN_POINT('Ctrl Pts',(-49.8533577168709,19.4137251539655,11.5));
#24326=CARTESIAN_POINT('Ctrl Pts',(-49.8197895303904,19.2181904935684,11.3977655520833));
#24327=CARTESIAN_POINT('Ctrl Pts',(-49.7863487149498,19.0233977693811,11.2969997378715));
#24328=CARTESIAN_POINT('',(-49.7079477042709,18.5667119425557,11.5));
#24329=CARTESIAN_POINT('Ctrl Pts',(-49.7863487149498,19.0233977693811,11.2969997378715));
#24330=CARTESIAN_POINT('Ctrl Pts',(-49.7421839478773,18.7661380351961,11.4654707447276));
#24331=CARTESIAN_POINT('Ctrl Pts',(-49.7079477042709,18.5667119425557,11.5));
#24332=CARTESIAN_POINT('',(-49.7079477042709,18.5667119425557,14.5));
#24333=CARTESIAN_POINT('Origin',(0.,0.,11.25));
#24334=CARTESIAN_POINT('',(-49.3474110662579,20.6659870574277,11.5));
#24335=CARTESIAN_POINT('Origin',(0.,0.,11.5));
#24336=CARTESIAN_POINT('',(-49.028064639274,20.9002167162411,11.2969997378715));
#24337=CARTESIAN_POINT('Ctrl Pts',(-49.028064639274,20.9002167162411,11.2969997378715));
#24338=CARTESIAN_POINT('Ctrl Pts',(-49.1874343451368,20.7833244992778,11.3977655520829));
#24339=CARTESIAN_POINT('Ctrl Pts',(-49.3474110662579,20.6659870574277,11.5));
#24340=CARTESIAN_POINT('',(-48.8290062914572,20.608933611151,11.));
#24341=CARTESIAN_POINT('Ctrl Pts',(-49.028064639274,20.9002167162411,11.2969997378715));
#24342=CARTESIAN_POINT('Ctrl Pts',(-48.9650785563254,20.7973785443115,11.1987310576086));
#24343=CARTESIAN_POINT('Ctrl Pts',(-48.8964856249514,20.699013451518,11.0971961933879));
#24344=CARTESIAN_POINT('Ctrl Pts',(-48.8290062914572,20.608933611151,11.));
#24345=CARTESIAN_POINT('',(-49.4408158756514,19.0946517525179,11.));
#24346=CARTESIAN_POINT('Origin',(0.,0.,11.));
#24347=CARTESIAN_POINT('Ctrl Pts',(-49.7863487149498,19.0233977693811,11.2969997378715));
#24348=CARTESIAN_POINT('Ctrl Pts',(-49.6696029216838,19.0536195497014,11.1987310576087));
#24349=CARTESIAN_POINT('Ctrl Pts',(-49.5519311610546,19.0767288219785,11.0971961933879));
#24350=CARTESIAN_POINT('Ctrl Pts',(-49.4408158756514,19.0946517525179,11.));
#24351=CARTESIAN_POINT('Origin',(0.,0.,14.5));
#24352=CARTESIAN_POINT('',(-49.3474110662579,20.6659870574277,24.2));
#24353=CARTESIAN_POINT('Origin',(0.,0.,24.2));
#24354=CARTESIAN_POINT('',(-49.3474110662579,20.6659870574277,14.5));
#24355=CARTESIAN_POINT('Origin',(-49.0009190529448,20.9201270734172,14.5));
#24356=CARTESIAN_POINT('',(-48.6544270396318,21.1742670894066,24.2));
#24357=CARTESIAN_POINT('',(-48.7795124544456,21.0825212248573,24.2));
#24358=CARTESIAN_POINT('',(-48.6544270396318,21.1742670894066,11.5));
#24359=CARTESIAN_POINT('',(-48.6544270396318,21.1742670894066,14.5));
#24360=CARTESIAN_POINT('Ctrl Pts',(-48.6544270396318,21.1742670894066,11.5));
#24361=CARTESIAN_POINT('Ctrl Pts',(-48.8175875368124,21.0545944569386,11.4654707447276));
#24362=CARTESIAN_POINT('Ctrl Pts',(-49.028064639274,20.9002167162411,11.2969997378715));
#24363=CARTESIAN_POINT('Origin',(-48.3346988609778,22.4164821240926,14.5));
#24364=CARTESIAN_POINT('',(-48.3776844341152,22.8440287338545,24.2));
#24365=CARTESIAN_POINT('',(-48.2917132878404,21.9889355143307,24.2));
#24366=CARTESIAN_POINT('',(-48.3072313028027,22.1432820590691,24.2));
#24367=CARTESIAN_POINT('',(-48.3776844341152,22.8440287338545,11.5));
#24368=CARTESIAN_POINT('',(-48.3776844341152,22.8440287338545,14.5));
#24369=CARTESIAN_POINT('',(-48.3380665247094,22.4499778554778,11.2969997378715));
#24370=CARTESIAN_POINT('Ctrl Pts',(-48.3776844341152,22.8440287338545,11.5));
#24371=CARTESIAN_POINT('Ctrl Pts',(-48.3578378264537,22.6466287877423,11.3977655520826));
#24372=CARTESIAN_POINT('Ctrl Pts',(-48.3380665247094,22.4499778554778,11.2969997378715));
#24373=CARTESIAN_POINT('',(-48.2917132878404,21.9889355143307,11.5));
#24374=CARTESIAN_POINT('Ctrl Pts',(-48.3380665247094,22.4499778554778,11.2969997378715));
#24375=CARTESIAN_POINT('Ctrl Pts',(-48.3119548726828,22.1902640146608,11.4654707447276));
#24376=CARTESIAN_POINT('Ctrl Pts',(-48.2917132878404,21.9889355143307,11.5));
#24377=CARTESIAN_POINT('',(-48.2917132878404,21.9889355143307,14.5));
#24378=CARTESIAN_POINT('Origin',(0.,0.,11.25));
#24379=CARTESIAN_POINT('',(-47.7856168695246,24.0579471360089,11.5));
#24380=CARTESIAN_POINT('Origin',(0.,0.,11.5));
#24381=CARTESIAN_POINT('',(-47.4507093193417,24.2693297424964,11.2969997378715));
#24382=CARTESIAN_POINT('Ctrl Pts',(-47.4507093193417,24.2693297424964,11.2969997378715));
#24383=CARTESIAN_POINT('Ctrl Pts',(-47.6178447974735,24.1638393378019,11.3977655520824));
#24384=CARTESIAN_POINT('Ctrl Pts',(-47.7856168695246,24.0579471360089,11.5));
#24385=CARTESIAN_POINT('',(-47.2724547499278,23.9648705799974,11.));
#24386=CARTESIAN_POINT('Ctrl Pts',(-47.4507093193417,24.2693297424964,11.2969997378715));
#24387=CARTESIAN_POINT('Ctrl Pts',(-47.3950502955656,24.1623483921435,11.1987310576087));
#24388=CARTESIAN_POINT('Ctrl Pts',(-47.3334860551377,24.0594381107558,11.0971961933879));
#24389=CARTESIAN_POINT('Ctrl Pts',(-47.2724547499278,23.9648705799974,11.));
#24390=CARTESIAN_POINT('',(-47.9884049594373,22.4969551150606,11.));
#24391=CARTESIAN_POINT('Origin',(0.,0.,11.));
#24392=CARTESIAN_POINT('Ctrl Pts',(-48.3380665247094,22.4499778554778,11.2969997378715));
#24393=CARTESIAN_POINT('Ctrl Pts',(-48.2194969535028,22.4719822421975,11.1987310576086));
#24394=CARTESIAN_POINT('Ctrl Pts',(-48.1004998140235,22.4868268543681,11.0971961933879));
#24395=CARTESIAN_POINT('Ctrl Pts',(-47.9884049594373,22.4969551150606,11.));
#24396=CARTESIAN_POINT('Origin',(0.,0.,14.5));
#24397=CARTESIAN_POINT('',(-47.7856168695246,24.0579471360089,24.2));
#24398=CARTESIAN_POINT('Origin',(0.,0.,24.2));
#24399=CARTESIAN_POINT('',(-47.7856168695246,24.0579471360089,14.5));
#24400=CARTESIAN_POINT('Origin',(-47.4222409819887,24.2872980186631,14.5));
#24401=CARTESIAN_POINT('',(-47.0588650944528,24.5166489013173,24.2));
#24402=CARTESIAN_POINT('',(-47.1900456754746,24.4338520425371,24.2));
#24403=CARTESIAN_POINT('',(-47.0588650944528,24.5166489013173,11.5));
#24404=CARTESIAN_POINT('',(-47.0588650944528,24.5166489013173,14.5));
#24405=CARTESIAN_POINT('Ctrl Pts',(-47.0588650944528,24.5166489013173,11.5));
#24406=CARTESIAN_POINT('Ctrl Pts',(-47.2299760817074,24.4086492863049,11.4654707447276));
#24407=CARTESIAN_POINT('Ctrl Pts',(-47.4507093193417,24.2693297424964,11.2969997378715));
#24408=CARTESIAN_POINT('Origin',(-46.653263217121,25.7335348523128,14.5));
#24409=CARTESIAN_POINT('',(-46.6663199357044,26.1630385020256,24.2));
#24410=CARTESIAN_POINT('',(-46.6402064985376,25.3040312025999,24.2));
#24411=CARTESIAN_POINT('',(-46.6449200416998,25.459084248916,24.2));
#24412=CARTESIAN_POINT('',(-46.6663199357044,26.1630385020256,11.5));
#24413=CARTESIAN_POINT('',(-46.6663199357044,26.1630385020257,14.5));
#24414=CARTESIAN_POINT('',(-46.6542861332861,25.7671839061264,11.2969997378715));
#24415=CARTESIAN_POINT('Ctrl Pts',(-46.6663199357044,26.1630385020256,11.5));
#24416=CARTESIAN_POINT('Ctrl Pts',(-46.6602915975399,25.9647349828969,11.3977655520838));
#24417=CARTESIAN_POINT('Ctrl Pts',(-46.6542861332861,25.7671839061264,11.2969997378715));
#24418=CARTESIAN_POINT('',(-46.6402064985376,25.3040312025999,11.5));
#24419=CARTESIAN_POINT('Ctrl Pts',(-46.6542861332861,25.7671839061264,11.2969997378715));
#24420=CARTESIAN_POINT('Ctrl Pts',(-46.6463548096495,25.5062812584035,11.4654707447276));
#24421=CARTESIAN_POINT('Ctrl Pts',(-46.6402064985376,25.3040312025999,11.5));
#24422=CARTESIAN_POINT('',(-46.6402064985376,25.3040312025999,14.5));
#24423=CARTESIAN_POINT('Origin',(0.,0.,11.25));
#24424=CARTESIAN_POINT('',(-45.9910159507968,27.3326993144394,11.5));
#24425=CARTESIAN_POINT('Origin',(0.,0.,11.5));
#24426=CARTESIAN_POINT('',(-45.6421789133341,27.5202050337906,11.2969997378715));
#24427=CARTESIAN_POINT('Ctrl Pts',(-45.6421789133341,27.5202050337906,11.2969997378715));
#24428=CARTESIAN_POINT('Ctrl Pts',(-45.8162658964882,27.4266303800113,11.3977655520832));
#24429=CARTESIAN_POINT('Ctrl Pts',(-45.9910159507968,27.3326993144394,11.5));
#24430=CARTESIAN_POINT('',(-45.4855965606673,27.2040531083184,11.));
#24431=CARTESIAN_POINT('Ctrl Pts',(-45.6421789133341,27.5202050337906,11.2969997378715));
#24432=CARTESIAN_POINT('Ctrl Pts',(-45.5941181138995,27.4096017073997,11.1987310576086));
#24433=CARTESIAN_POINT('Ctrl Pts',(-45.5398824992087,27.3026476059643,11.0971961933879));
#24434=CARTESIAN_POINT('Ctrl Pts',(-45.4855965606673,27.2040531083184,11.));
#24435=CARTESIAN_POINT('',(-46.3021993580384,25.7896555736688,11.));
#24436=CARTESIAN_POINT('Origin',(0.,0.,11.));
#24437=CARTESIAN_POINT('Ctrl Pts',(-46.6542861332861,25.7671839061264,11.2969997378715));
#24438=CARTESIAN_POINT('Ctrl Pts',(-46.5344704431712,25.7808636960853,11.1987310576086));
#24439=CARTESIAN_POINT('Ctrl Pts',(-46.4147276669438,25.787371326691,11.0971961933879));
#24440=CARTESIAN_POINT('Ctrl Pts',(-46.3021993580384,25.7896555736688,11.));
#24441=CARTESIAN_POINT('Origin',(0.,0.,14.5));
#24442=CARTESIAN_POINT('',(-45.9910159507968,27.3326993144394,24.2));
#24443=CARTESIAN_POINT('Origin',(0.,0.,24.2));
#24444=CARTESIAN_POINT('',(-45.9910159507968,27.3326993144394,14.5));
#24445=CARTESIAN_POINT('Origin',(-45.6125265198356,27.5361436893125,14.5));
#24446=CARTESIAN_POINT('',(-45.2340370888744,27.7395880641857,24.2));
#24447=CARTESIAN_POINT('',(-45.3706737374995,27.6661435891479,24.2));
#24448=CARTESIAN_POINT('',(-45.2340370888744,27.7395880641857,11.5));
#24449=CARTESIAN_POINT('',(-45.2340370888744,27.7395880641857,14.5));
#24450=CARTESIAN_POINT('Ctrl Pts',(-45.2340370888744,27.7395880641857,11.5));
#24451=CARTESIAN_POINT('Ctrl Pts',(-45.412264930673,27.6437876298971,11.4654707447275));
#24452=CARTESIAN_POINT('Ctrl Pts',(-45.6421789133341,27.5202050337906,11.2969997378715));
#24453=CARTESIAN_POINT('Origin',(-44.74453756444,28.9252163854584,14.5));
#24454=CARTESIAN_POINT('',(-44.727601817449,29.3545845765144,24.2));
#24455=CARTESIAN_POINT('',(-44.7614733114311,28.4958481944023,24.2));
#24456=CARTESIAN_POINT('',(-44.7553594188847,28.6508523394404,24.2));
#24457=CARTESIAN_POINT('',(-44.727601817449,29.3545845765144,11.5));
#24458=CARTESIAN_POINT('',(-44.727601817449,29.3545845765144,14.5));
#24459=CARTESIAN_POINT('',(-44.7432107494939,28.9588548268927,11.2969997378715));
#24460=CARTESIAN_POINT('Ctrl Pts',(-44.727601817449,29.3545845765144,11.5));
#24461=CARTESIAN_POINT('Ctrl Pts',(-44.7354211182388,29.1563435991768,11.3977655520828));
#24462=CARTESIAN_POINT('Ctrl Pts',(-44.7432107494939,28.9588548268927,11.2969997378715));
#24463=CARTESIAN_POINT('',(-44.7614733114311,28.4958481944023,11.5));
#24464=CARTESIAN_POINT('Ctrl Pts',(-44.7432107494939,28.9588548268927,11.2969997378715));
#24465=CARTESIAN_POINT('Ctrl Pts',(-44.7534983948587,28.6980344637377,11.4654707447276));
#24466=CARTESIAN_POINT('Ctrl Pts',(-44.7614733114311,28.4958481944023,11.5));
#24467=CARTESIAN_POINT('',(-44.7614733114311,28.4958481944023,14.5));
#24468=CARTESIAN_POINT('Origin',(0.,0.,11.25));
#24469=CARTESIAN_POINT('',(-43.9723514253571,30.4742893292837,11.5));
#24470=CARTESIAN_POINT('Origin',(0.,0.,11.5));
#24471=CARTESIAN_POINT('',(-43.6112843995965,30.6370046524817,11.2969997378715));
#24472=CARTESIAN_POINT('Ctrl Pts',(-43.6112843995965,30.6370046524817,11.2969997378715));
#24473=CARTESIAN_POINT('Ctrl Pts',(-43.7914747534883,30.5558016359257,11.397765552083));
#24474=CARTESIAN_POINT('Ctrl Pts',(-43.9723514253571,30.4742893292837,11.5));
#24475=CARTESIAN_POINT('',(-43.4771371171594,30.3107002244375,11.));
#24476=CARTESIAN_POINT('Ctrl Pts',(-43.6112843995965,30.6370046524817,11.2969997378715));
#24477=CARTESIAN_POINT('Ctrl Pts',(-43.5710559718872,30.5233181983411,11.1987310576087));
#24478=CARTESIAN_POINT('Ctrl Pts',(-43.5244132133966,30.4128413464891,11.0971961933879));
#24479=CARTESIAN_POINT('Ctrl Pts',(-43.4771371171594,30.3107002244375,11.));
#24480=CARTESIAN_POINT('',(-44.390414095648,28.9567114226892,11.));
#24481=CARTESIAN_POINT('Origin',(0.,0.,11.));
#24482=CARTESIAN_POINT('Ctrl Pts',(-44.7432107494939,28.9588548268927,11.2969997378715));
#24483=CARTESIAN_POINT('Ctrl Pts',(-44.6227326704691,28.9641433735292,11.1987310576086));
#24484=CARTESIAN_POINT('Ctrl Pts',(-44.5028276322629,28.9622823180478,11.0971961933879));
#24485=CARTESIAN_POINT('Ctrl Pts',(-44.390414095648,28.9567114226892,11.));
#24486=CARTESIAN_POINT('Origin',(0.,0.,14.5));
#24487=CARTESIAN_POINT('',(-43.9723514253571,30.4742893292837,24.2));
#24488=CARTESIAN_POINT('Origin',(0.,0.,24.2));
#24489=CARTESIAN_POINT('',(-43.9723514253571,30.4742893292837,14.5));
#24490=CARTESIAN_POINT('Origin',(-43.5805924134327,30.6508360358314,14.5));
#24491=CARTESIAN_POINT('',(-43.1888334015084,30.827382742379,24.2));
#24492=CARTESIAN_POINT('',(-43.3302604377194,30.7636484651835,24.2));
#24493=CARTESIAN_POINT('',(-43.1888334015084,30.827382742379,11.5));
#24494=CARTESIAN_POINT('',(-43.1888334015084,30.827382742379,14.5));
#24495=CARTESIAN_POINT('Ctrl Pts',(-43.1888334015084,30.827382742379,11.5));
#24496=CARTESIAN_POINT('Ctrl Pts',(-43.3733097897212,30.7442482189004,11.4654707447276));
#24497=CARTESIAN_POINT('Ctrl Pts',(-43.6112843995965,30.6370046524817,11.2969997378715));
#24498=CARTESIAN_POINT('Origin',(-42.6178210224504,31.9759771719264,14.5));
#24499=CARTESIAN_POINT('',(-42.5709753191419,32.4031180656586,24.2));
#24500=CARTESIAN_POINT('',(-42.6646667257588,31.5488362781942,24.2));
#24501=CARTESIAN_POINT('',(-42.6477551837739,31.7030363573407,24.2));
#24502=CARTESIAN_POINT('',(-42.5709753191419,32.4031180656586,11.5));
#24503=CARTESIAN_POINT('',(-42.5709753191419,32.4031180656586,14.5));
#24504=CARTESIAN_POINT('',(-42.614150940502,32.0094411178763,11.2969997378715));
#24505=CARTESIAN_POINT('Ctrl Pts',(-42.5709753191419,32.4031180656586,11.5));
#24506=CARTESIAN_POINT('Ctrl Pts',(-42.5926041640386,32.2059054402286,11.3977655520829));
#24507=CARTESIAN_POINT('Ctrl Pts',(-42.614150940502,32.0094411178763,11.2969997378715));
#24508=CARTESIAN_POINT('',(-42.6646667257588,31.5488362781942,11.5));
#24509=CARTESIAN_POINT('Ctrl Pts',(-42.614150940502,32.0094411178763,11.2969997378715));
#24510=CARTESIAN_POINT('Ctrl Pts',(-42.642607434494,31.7499737298808,11.4654707447276));
#24511=CARTESIAN_POINT('Ctrl Pts',(-42.6646667257588,31.5488362781942,11.5));
#24512=CARTESIAN_POINT('',(-42.6646667257588,31.5488362781942,14.5));
#24513=CARTESIAN_POINT('Origin',(0.,0.,11.25));
#24514=CARTESIAN_POINT('',(-41.7394580238585,33.4674116697804,11.5));
#24515=CARTESIAN_POINT('Origin',(0.,0.,11.5));
#24516=CARTESIAN_POINT('',(-41.3679200920551,33.6045438641268,11.2969997378715));
#24517=CARTESIAN_POINT('Ctrl Pts',(-41.3679200920551,33.6045438641268,11.2969997378715));
#24518=CARTESIAN_POINT('Ctrl Pts',(-41.5533359473934,33.5361080977281,11.397765552083));
#24519=CARTESIAN_POINT('Ctrl Pts',(-41.7394580238585,33.4674116697804,11.5));
#24520=CARTESIAN_POINT('',(-41.2568614319233,33.2696766558841,11.));
#24521=CARTESIAN_POINT('Ctrl Pts',(-41.3679200920551,33.6045438641268,11.2969997378715));
#24522=CARTESIAN_POINT('Ctrl Pts',(-41.3357200249272,33.4883281512133,11.1987310576087));
#24523=CARTESIAN_POINT('Ctrl Pts',(-41.2968973614676,33.3748667810619,11.097196193388));
#24524=CARTESIAN_POINT('Ctrl Pts',(-41.2568614319233,33.2696766558841,11.));
#24525=CARTESIAN_POINT('',(-42.2623631978924,31.9826930843766,11.));
#24526=CARTESIAN_POINT('Origin',(0.,0.,11.));
#24527=CARTESIAN_POINT('Ctrl Pts',(-42.614150940502,32.0094411178763,11.2969997378715));
#24528=CARTESIAN_POINT('Ctrl Pts',(-42.4935974296579,32.0063126559227,11.1987310576087));
#24529=CARTESIAN_POINT('Ctrl Pts',(-42.3741142947661,31.9960919812296,11.0971961933879));
#24530=CARTESIAN_POINT('Ctrl Pts',(-42.2623631978924,31.9826930843766,11.));
#24531=CARTESIAN_POINT('Origin',(0.,0.,14.5));
#24532=CARTESIAN_POINT('',(-41.7394580238585,33.4674116697804,24.2));
#24533=CARTESIAN_POINT('Origin',(0.,0.,24.2));
#24534=CARTESIAN_POINT('',(-41.7394580238585,33.4674116697804,14.5));
#24535=CARTESIAN_POINT('Origin',(-41.3363380414976,33.6162005901948,14.5));
#24536=CARTESIAN_POINT('',(-40.9332180591366,33.7649895106092,24.2));
#24537=CARTESIAN_POINT('',(-41.0787464646293,33.7112759382477,24.2));
#24538=CARTESIAN_POINT('',(-40.9332180591366,33.7649895106092,11.5));
#24539=CARTESIAN_POINT('',(-40.9332180591366,33.7649895106092,14.5));
#24540=CARTESIAN_POINT('Ctrl Pts',(-40.9332180591366,33.7649895106092,11.5));
#24541=CARTESIAN_POINT('Ctrl Pts',(-41.1230442433438,33.6949259209822,11.4654707447276));
#24542=CARTESIAN_POINT('Ctrl Pts',(-41.3679200920551,33.6045438641268,11.2969997378715));
#24543=CARTESIAN_POINT('Origin',(-40.2834747403676,34.870954211827,14.5));
#24544=CARTESIAN_POINT('',(-40.2069473082993,35.2937868207372,24.2));
#24545=CARTESIAN_POINT('',(-40.3600021724359,34.4481216029168,24.2));
#24546=CARTESIAN_POINT('',(-40.332375372345,34.600766368886,24.2));
#24547=CARTESIAN_POINT('',(-40.2069473082993,35.2937868207372,11.5));
#24548=CARTESIAN_POINT('',(-40.2069473082993,35.2937868207372,14.5));
#24549=CARTESIAN_POINT('',(-40.2774792716874,34.9040806293114,11.2969997378715));
#24550=CARTESIAN_POINT('Ctrl Pts',(-40.2069473082993,35.2937868207372,11.5));
#24551=CARTESIAN_POINT('Ctrl Pts',(-40.2422803237447,35.098563347302,11.3977655520829));
#24552=CARTESIAN_POINT('Ctrl Pts',(-40.2774792716874,34.9040806293114,11.2969997378715));
#24553=CARTESIAN_POINT('',(-40.3600021724359,34.4481216029168,11.5));
#24554=CARTESIAN_POINT('Ctrl Pts',(-40.2774792716874,34.9040806293114,11.2969997378715));
#24555=CARTESIAN_POINT('Ctrl Pts',(-40.3239659771285,34.6472303155083,11.4654707447276));
#24556=CARTESIAN_POINT('Ctrl Pts',(-40.3600021724359,34.4481216029168,11.5));
#24557=CARTESIAN_POINT('',(-40.3600021724359,34.4481216029168,14.5));
#24558=CARTESIAN_POINT('Origin',(0.,0.,11.25));
#24559=CARTESIAN_POINT('',(-39.3032141785034,36.2974841447543,11.5));
#24560=CARTESIAN_POINT('Origin',(0.,0.,11.5));
#24561=CARTESIAN_POINT('',(-38.923015436114,36.4083651159827,11.2969997378715));
#24562=CARTESIAN_POINT('Ctrl Pts',(-38.923015436114,36.4083651159827,11.2969997378715));
#24563=CARTESIAN_POINT('Ctrl Pts',(-39.11275346549,36.353030011916,11.3977655520832));
#24564=CARTESIAN_POINT('Ctrl Pts',(-39.3032141785034,36.2974841447543,11.5));
#24565=CARTESIAN_POINT('',(-38.835586464916,36.0665665669195,11.));
#24566=CARTESIAN_POINT('Ctrl Pts',(-38.923015436114,36.4083651159827,11.2969997378715));
#24567=CARTESIAN_POINT('Ctrl Pts',(-38.8990006050577,36.2901863355677,11.1987310576087));
#24568=CARTESIAN_POINT('Ctrl Pts',(-38.868187176743,36.1742932195071,11.0971961933879));
#24569=CARTESIAN_POINT('Ctrl Pts',(-38.835586464916,36.0665665669195,11.));
#24570=CARTESIAN_POINT('',(-39.9284143148345,34.8528582802461,11.));
#24571=CARTESIAN_POINT('Origin',(0.,0.,11.));
#24572=CARTESIAN_POINT('Ctrl Pts',(-40.2774792716874,34.9040806293114,11.2969997378715));
#24573=CARTESIAN_POINT('Ctrl Pts',(-40.1574376536108,34.8925504003199,11.1987310576087));
#24574=CARTESIAN_POINT('Ctrl Pts',(-40.0389585318564,34.8740199005147,11.0971961933879));
#24575=CARTESIAN_POINT('Ctrl Pts',(-39.9284143148345,34.8528582802461,11.));
#24576=CARTESIAN_POINT('Origin',(0.,0.,14.5));
#24577=CARTESIAN_POINT('',(-39.3032141785034,36.2974841447543,24.2));
#24578=CARTESIAN_POINT('Origin',(0.,0.,24.2));
#24579=CARTESIAN_POINT('',(-39.3032141785034,36.2974841447543,14.5));
#24580=CARTESIAN_POINT('Origin',(-38.8906971857384,36.4177903943714,14.5));
#24581=CARTESIAN_POINT('',(-38.4781801929734,36.5380966439885,24.2));
#24582=CARTESIAN_POINT('',(-38.6271009679847,36.4946654635864,24.2));
#24583=CARTESIAN_POINT('',(-38.4781801929734,36.5380966439885,11.5));
#24584=CARTESIAN_POINT('',(-38.4781801929734,36.5380966439885,14.5));
#24585=CARTESIAN_POINT('Ctrl Pts',(-38.4781801929734,36.5380966439885,11.5));
#24586=CARTESIAN_POINT('Ctrl Pts',(-38.6724313590868,36.481445330979,11.4654707447276));
#24587=CARTESIAN_POINT('Ctrl Pts',(-38.923015436114,36.4083651159827,11.2969997378715));
#24588=CARTESIAN_POINT('Origin',(-37.7528714186305,37.5960434680237,14.5));
#24589=CARTESIAN_POINT('',(-37.6470350917587,38.0125077941444,24.2));
#24590=CARTESIAN_POINT('',(-37.8587077455022,37.179579141903,24.2));
#24591=CARTESIAN_POINT('',(-37.8205002822982,37.329924924739,24.2));
#24592=CARTESIAN_POINT('',(-37.6470350917587,38.0125077941444,11.5));
#24593=CARTESIAN_POINT('',(-37.6470350917587,38.0125077941444,14.5));
#24594=CARTESIAN_POINT('',(-37.7445797725392,37.6286709684663,11.2969997378715));
#24595=CARTESIAN_POINT('Ctrl Pts',(-37.6470350917587,38.0125077941444,11.5));
#24596=CARTESIAN_POINT('Ctrl Pts',(-37.6959001388532,37.8202245818431,11.397765552083));
#24597=CARTESIAN_POINT('Ctrl Pts',(-37.7445797725392,37.6286709684663,11.2969997378715));
#24598=CARTESIAN_POINT('',(-37.8587077455022,37.179579141903,11.5));
#24599=CARTESIAN_POINT('Ctrl Pts',(-37.7445797725392,37.6286709684663,11.2969997378715));
#24600=CARTESIAN_POINT('Ctrl Pts',(-37.8088702108732,37.375689077766,11.4654707447276));
#24601=CARTESIAN_POINT('Ctrl Pts',(-37.8587077455022,37.179579141903,11.5));
#24602=CARTESIAN_POINT('',(-37.8587077455022,37.179579141903,14.5));
#24603=CARTESIAN_POINT('Origin',(0.,0.,11.25));
#24604=CARTESIAN_POINT('',(-36.6754890244158,38.9507189255854,11.5));
#24605=CARTESIAN_POINT('Origin',(0.,0.,11.5));
#24606=CARTESIAN_POINT('',(-36.288481761496,39.0348084727497,11.2969997378715));
#24607=CARTESIAN_POINT('Ctrl Pts',(-36.288481761496,39.0348084727497,11.2969997378715));
#24608=CARTESIAN_POINT('Ctrl Pts',(-36.4816175803016,38.99284361808,11.3977655520827));
#24609=CARTESIAN_POINT('Ctrl Pts',(-36.6754890244158,38.9507189255854,11.5));
#24610=CARTESIAN_POINT('',(-36.2251084243911,38.6877437910394,11.));
#24611=CARTESIAN_POINT('Ctrl Pts',(-36.288481761496,39.0348084727497,11.2969997378715));
#24612=CARTESIAN_POINT('Ctrl Pts',(-36.2727691643543,38.9152423799721,11.1987310576087));
#24613=CARTESIAN_POINT('Ctrl Pts',(-36.2501150911098,38.7974821376142,11.0971961933879));
#24614=CARTESIAN_POINT('Ctrl Pts',(-36.2251084243911,38.6877437910394,11.));
#24615=CARTESIAN_POINT('',(-37.3999382108249,37.5532238539712,11.));
#24616=CARTESIAN_POINT('Origin',(0.,0.,11.));
#24617=CARTESIAN_POINT('Ctrl Pts',(-37.7445797725392,37.6286709684663,11.2969997378715));
#24618=CARTESIAN_POINT('Ctrl Pts',(-37.6256348779268,37.6087951465536,11.1987310576086));
#24619=CARTESIAN_POINT('Ctrl Pts',(-37.5087369876814,37.5820451003687,11.0971961933879));
#24620=CARTESIAN_POINT('Ctrl Pts',(-37.399938210825,37.5532238539712,11.));
#24621=CARTESIAN_POINT('Origin',(0.,0.,14.5));
#24622=CARTESIAN_POINT('',(-36.6754890244158,38.9507189255854,24.2));
#24623=CARTESIAN_POINT('Origin',(0.,0.,24.2));
#24624=CARTESIAN_POINT('',(-36.6754890244158,38.9507189255854,14.5));
#24625=CARTESIAN_POINT('Origin',(-36.2555847625695,39.0419563844502,14.5));
#24626=CARTESIAN_POINT('',(-35.8356805007232,39.1331938433149,24.2));
#24627=CARTESIAN_POINT('',(-35.9872681182067,39.1002566472175,24.2));
#24628=CARTESIAN_POINT('',(-35.8356805007232,39.1331938433149,11.5));
#24629=CARTESIAN_POINT('',(-35.8356805007232,39.1331938433149,14.5));
#24630=CARTESIAN_POINT('Ctrl Pts',(-35.8356805007232,39.1331938433149,11.5));
#24631=CARTESIAN_POINT('Ctrl Pts',(-36.0334102765874,39.0902308064254,11.4654707447276));
#24632=CARTESIAN_POINT('Ctrl Pts',(-36.288481761496,39.0348084727497,11.2969997378715));
#24633=CARTESIAN_POINT('Origin',(-35.8654005008348,39.8325626455883,11.25));
#24634=CARTESIAN_POINT('',(-35.1729694999764,39.729901508588,11.5));
#24635=CARTESIAN_POINT('Origin',(-35.8654005008348,39.8325626455883,11.5));
#24636=CARTESIAN_POINT('',(-35.027792474811,40.1699382050837,11.2969997378714));
#24637=CARTESIAN_POINT('Ctrl Pts',(-35.027792474811,40.1699382050837,11.2969997378714));
#24638=CARTESIAN_POINT('Ctrl Pts',(-35.1095734294849,39.9220572398278,11.4654707447275));
#24639=CARTESIAN_POINT('Ctrl Pts',(-35.1729694999764,39.729901508588,11.5));
#24640=CARTESIAN_POINT('',(-34.6892533672809,40.0706338959167,11.));
#24641=CARTESIAN_POINT('Ctrl Pts',(-34.6892533672809,40.0706338959167,11.));
#24642=CARTESIAN_POINT('Ctrl Pts',(-34.7645593265508,40.0963245531492,11.0687122343714));
#24643=CARTESIAN_POINT('Ctrl Pts',(-34.841627036511,40.1204761473162,11.1374591885178));
#24644=CARTESIAN_POINT('Ctrl Pts',(-34.955624113946,40.1519342014003,11.2360127801162));
#24645=CARTESIAN_POINT('Ctrl Pts',(-34.9916111096869,40.161260817967,11.2666805180049));
#24646=CARTESIAN_POINT('Ctrl Pts',(-35.027792474811,40.1699382050837,11.2969997378714));
#24647=CARTESIAN_POINT('Origin',(-35.8654005008348,39.8325626455883,11.));
#24648=CARTESIAN_POINT('Origin',(0.,0.,11.25));
#24649=CARTESIAN_POINT('Origin',(0.,0.,11.));
#24650=CARTESIAN_POINT('Origin',(0.,0.,11.5));
#24651=CARTESIAN_POINT('Origin',(0.,0.,11.25));
#24652=CARTESIAN_POINT('Origin',(0.,0.,11.));
#24653=CARTESIAN_POINT('Origin',(0.,0.,11.5));
#24654=CARTESIAN_POINT('Origin',(0.,0.,11.25));
#24655=CARTESIAN_POINT('',(-51.0861504520717,-15.8888398565878,11.5));
#24656=CARTESIAN_POINT('Origin',(0.,0.,11.5));
#24657=CARTESIAN_POINT('',(-50.8820099961117,-15.0540332165161,11.0622545443405));
#24658=CARTESIAN_POINT('Ctrl Pts',(-51.0861504520717,-15.8888398565878,
11.5));
#24659=CARTESIAN_POINT('Ctrl Pts',(-50.9836609313633,-15.4697218918374,
11.2776618075213));
#24660=CARTESIAN_POINT('Ctrl Pts',(-50.8820099961117,-15.0540332165161,
11.0622545443405));
#24661=CARTESIAN_POINT('',(-50.8468800894551,-14.9530861419499,11.));
#24662=CARTESIAN_POINT('Ctrl Pts',(-50.8468800894551,-14.9530861419499,
11.));
#24663=CARTESIAN_POINT('Ctrl Pts',(-50.8563919627033,-14.9890630627436,
11.0192757561174));
#24664=CARTESIAN_POINT('Ctrl Pts',(-50.86845859598,-15.0229660136113,11.0404460254343));
#24665=CARTESIAN_POINT('Ctrl Pts',(-50.8820099961117,-15.0540332165161,
11.0622545443405));
#24666=CARTESIAN_POINT('Origin',(0.,0.,11.));
#24667=CARTESIAN_POINT('Origin',(0.,0.,11.));
#24668=CARTESIAN_POINT('',(-51.0445282617143,-14.2638050512144,11.));
#24669=CARTESIAN_POINT('Origin',(-51.5236269022939,-14.7741622717911,11.));
#24670=CARTESIAN_POINT('',(-51.766094205967,-11.3697621197168,11.));
#24671=CARTESIAN_POINT('Origin',(0.,0.,11.));
#24672=CARTESIAN_POINT('',(-51.9151790989041,-10.6683728435365,11.));
#24673=CARTESIAN_POINT('Origin',(-52.428711399332,-11.1440666278319,11.));
#24674=CARTESIAN_POINT('',(-52.4331091150171,-7.73104575932095,11.));
#24675=CARTESIAN_POINT('Origin',(0.,0.,11.));
#24676=CARTESIAN_POINT('',(-52.5329044020197,-7.02096539574591,11.));
#24677=CARTESIAN_POINT('Origin',(-53.0783684845482,-7.45967821145951,11.));
#24678=CARTESIAN_POINT('',(-52.8446751870164,-4.05466452110769,11.));
#24679=CARTESIAN_POINT('Origin',(0.,0.,11.));
#24680=CARTESIAN_POINT('',(-52.8946946754777,-3.33935251029225,11.));
#24681=CARTESIAN_POINT('Origin',(-53.4694330939266,-3.73894699268512,11.));
#24682=CARTESIAN_POINT('',(-52.9987873134328,-0.358529364921027,11.));
#24683=CARTESIAN_POINT('Origin',(0.,0.,11.));
#24684=CARTESIAN_POINT('',(-52.9987873134328,0.35852936492104,11.));
#24685=CARTESIAN_POINT('Origin',(-53.6,6.56410684342981E-15,11.));
#24686=CARTESIAN_POINT('',(-52.8946946754776,3.33935251029228,11.));
#24687=CARTESIAN_POINT('Origin',(0.,0.,11.));
#24688=CARTESIAN_POINT('',(-52.8446751870164,4.05466452110769,11.));
#24689=CARTESIAN_POINT('Origin',(-53.4694330939266,3.73894699268513,11.));
#24690=CARTESIAN_POINT('Origin',(0.,0.,11.));
#24691=CARTESIAN_POINT('Origin',(-52.428711399332,11.1440666278319,11.));
#24692=CARTESIAN_POINT('Origin',(-51.5236269022939,14.7741622717912,11.));
#24693=CARTESIAN_POINT('Origin',(-50.3675244741247,18.3322796822559,11.));
#24694=CARTESIAN_POINT('Origin',(-48.9660365296434,21.8010840688629,11.));
#24695=CARTESIAN_POINT('Origin',(-47.3259909772385,25.1636757653237,11.));
#24696=CARTESIAN_POINT('Origin',(-45.4553779539844,28.4036725628998,11.));
#24697=CARTESIAN_POINT('Origin',(-43.3633108984972,31.5052895228766,11.));
#24698=CARTESIAN_POINT('Origin',(-41.0599821511772,34.4534158791985,11.));
#24699=CARTESIAN_POINT('Origin',(-38.5566132981517,37.2336886566023,11.));
#24700=CARTESIAN_POINT('',(-33.4381452969578,41.1204382162877,11.));
#24701=CARTESIAN_POINT('Origin',(0.,0.,11.));
#24702=CARTESIAN_POINT('',(-31.809565968283,42.3928238374073,11.));
#24703=CARTESIAN_POINT('Origin',(-32.9994550774553,42.2373763933203,11.));
#24704=CARTESIAN_POINT('',(-30.4882748868283,43.3527979999583,11.));
#24705=CARTESIAN_POINT('Origin',(0.,0.,11.));
#24706=CARTESIAN_POINT('',(-28.774905561374,44.5084802024739,11.));
#24707=CARTESIAN_POINT('Origin',(-29.972739626032,44.4364138889502,11.));
#24708=CARTESIAN_POINT('',(-27.3898686661209,45.3739473095812,11.));
#24709=CARTESIAN_POINT('Origin',(0.,0.,11.));
#24710=CARTESIAN_POINT('',(-25.6000567070134,46.4072957259707,11.));
#24711=CARTESIAN_POINT('Origin',(-26.8,46.4189616428459,11.));
#24712=CARTESIAN_POINT('',(-24.1580217584921,47.174039308885,11.));
#24713=CARTESIAN_POINT('Origin',(0.,0.,11.));
#24714=CARTESIAN_POINT('',(-22.300486949685,48.0800195695356,11.));
#24715=CARTESIAN_POINT('Origin',(-23.4966934678946,48.1753608816354,11.));
#24716=CARTESIAN_POINT('',(-20.8084793972118,48.7443041305937,11.));
#24717=CARTESIAN_POINT('Origin',(0.,0.,11.));
#24718=CARTESIAN_POINT('',(-18.8922714615747,49.5185023907445,11.));
#24719=CARTESIAN_POINT('Origin',(-20.0789134070929,49.6970546047798,11.));
#24720=CARTESIAN_POINT('',(-17.3575602159692,50.0770916023385,11.));
#24721=CARTESIAN_POINT('Origin',(0.,0.,11.));
#24722=CARTESIAN_POINT('',(-15.3920147259482,50.7157360458881,11.));
#24723=CARTESIAN_POINT('Origin',(-16.5633108984972,50.9766292734202,11.));
#24724=CARTESIAN_POINT('',(-13.8220767461304,51.1659085175284,11.));
#24725=CARTESIAN_POINT('Origin',(0.,0.,11.));
#24726=CARTESIAN_POINT('',(-11.8167696417768,51.6658877329441,11.));
#24727=CARTESIAN_POINT('Origin',(-12.9670136041422,52.0078509283934,11.));
#24728=CARTESIAN_POINT('',(-10.2192535077747,52.0054502696,11.));
#24729=CARTESIAN_POINT('Origin',(0.,0.,11.));
#24730=CARTESIAN_POINT('',(-8.18395444372813,52.3643284084021,11.));
#24731=CARTESIAN_POINT('Origin',(-9.30754232294747,52.7856955614544,11.));
#24732=CARTESIAN_POINT('',(-6.56664309356487,52.5916266955277,11.));
#24733=CARTESIAN_POINT('Origin',(0.,0.,11.));
#24734=CARTESIAN_POINT('Origin',(-5.60272563114623,53.3063735917395,11.));
#24735=CARTESIAN_POINT('',(-1.49132004456261,52.9790143785696,11.));
#24736=CARTESIAN_POINT('Origin',(-1.87061302325405,53.5673483282235,11.));
#24737=CARTESIAN_POINT('',(1.49132004456262,52.9790143785696,11.));
#24738=CARTESIAN_POINT('Origin',(0.,0.,11.));
#24739=CARTESIAN_POINT('',(2.2079419616008,52.953989389792,11.));
#24740=CARTESIAN_POINT('Origin',(1.87061302325406,53.5673483282235,11.));
#24741=CARTESIAN_POINT('',(4.51126784227787,52.8076553394982,11.));
#24742=CARTESIAN_POINT('Origin',(0.,0.,11.));
#24743=CARTESIAN_POINT('',(6.56664309356487,52.5916266955277,11.));
#24744=CARTESIAN_POINT('Origin',(5.60272563114623,53.3063735917395,11.));
#24745=CARTESIAN_POINT('',(8.18395444372813,52.3643284084021,11.));
#24746=CARTESIAN_POINT('Origin',(0.,0.,11.));
#24747=CARTESIAN_POINT('',(10.2192535077747,52.0054502696,11.));
#24748=CARTESIAN_POINT('Origin',(9.30754232294747,52.7856955614544,11.));
#24749=CARTESIAN_POINT('',(11.8167696417768,51.6658877329441,11.));
#24750=CARTESIAN_POINT('Origin',(0.,0.,11.));
#24751=CARTESIAN_POINT('',(13.8220767461304,51.1659085175284,11.));
#24752=CARTESIAN_POINT('Origin',(12.9670136041422,52.0078509283934,11.));
#24753=CARTESIAN_POINT('',(15.3920147259482,50.7157360458881,11.));
#24754=CARTESIAN_POINT('Origin',(0.,0.,11.));
#24755=CARTESIAN_POINT('',(17.3575602159693,50.0770916023385,11.));
#24756=CARTESIAN_POINT('Origin',(16.5633108984972,50.9766292734202,11.));
#24757=CARTESIAN_POINT('',(18.8922714615747,49.5185023907445,11.));
#24758=CARTESIAN_POINT('Origin',(0.,0.,11.));
#24759=CARTESIAN_POINT('',(20.8084793972118,48.7443041305937,11.));
#24760=CARTESIAN_POINT('Origin',(20.0789134070929,49.6970546047798,11.));
#24761=CARTESIAN_POINT('',(22.300486949685,48.0800195695356,11.));
#24762=CARTESIAN_POINT('Origin',(0.,0.,11.));
#24763=CARTESIAN_POINT('',(24.1580217584921,47.1740393088849,11.));
#24764=CARTESIAN_POINT('Origin',(23.4966934678946,48.1753608816354,11.));
#24765=CARTESIAN_POINT('',(25.6000567070134,46.4072957259707,11.));
#24766=CARTESIAN_POINT('Origin',(0.,0.,11.));
#24767=CARTESIAN_POINT('',(27.3898686661209,45.3739473095812,11.));
#24768=CARTESIAN_POINT('Origin',(26.8,46.4189616428459,11.));
#24769=CARTESIAN_POINT('',(28.774905561374,44.5084802024738,11.));
#24770=CARTESIAN_POINT('Origin',(0.,0.,11.));
#24771=CARTESIAN_POINT('',(30.4882748868283,43.3527979999583,11.));
#24772=CARTESIAN_POINT('Origin',(29.972739626032,44.4364138889502,11.));
#24773=CARTESIAN_POINT('',(32.3467865928173,41.9843470488554,11.));
#24774=CARTESIAN_POINT('Origin',(0.,0.,11.));
#24775=CARTESIAN_POINT('',(32.9118365829004,41.5428816133457,11.));
#24776=CARTESIAN_POINT('Origin',(32.9994550774553,42.2373763933203,11.));
#24777=CARTESIAN_POINT('',(34.6892533672809,40.0706338959167,11.));
#24778=CARTESIAN_POINT('Origin',(0.,0.,11.));
#24779=CARTESIAN_POINT('',(36.2251084243911,38.6877437910394,11.));
#24780=CARTESIAN_POINT('Origin',(35.8654005008348,39.8325626455883,11.));
#24781=CARTESIAN_POINT('',(37.8750816598377,37.0739556732301,11.));
#24782=CARTESIAN_POINT('Origin',(0.,0.,11.));
#24783=CARTESIAN_POINT('',(38.3731925086332,36.5581467896744,11.));
#24784=CARTESIAN_POINT('Origin',(38.5566132981517,37.2336886566023,11.));
#24785=CARTESIAN_POINT('',(39.9284143148345,34.8528582802461,11.));
#24786=CARTESIAN_POINT('Origin',(0.,0.,11.));
#24787=CARTESIAN_POINT('',(41.2568614319233,33.2696766558841,11.));
#24788=CARTESIAN_POINT('Origin',(41.0599821511772,34.4534158791985,11.));
#24789=CARTESIAN_POINT('',(42.2623631978924,31.9826930843766,11.));
#24790=CARTESIAN_POINT('Origin',(0.,0.,11.));
#24791=CARTESIAN_POINT('',(43.4771371171594,30.3107002244375,11.));
#24792=CARTESIAN_POINT('Origin',(43.3633108984972,31.5052895228766,11.));
#24793=CARTESIAN_POINT('',(44.390414095648,28.9567114226892,11.));
#24794=CARTESIAN_POINT('Origin',(0.,0.,11.));
#24795=CARTESIAN_POINT('',(45.4855965606673,27.2040531083184,11.));
#24796=CARTESIAN_POINT('Origin',(45.4553779539844,28.4036725628998,11.));
#24797=CARTESIAN_POINT('',(46.3021993580384,25.7896555736688,11.));
#24798=CARTESIAN_POINT('Origin',(0.,0.,11.));
#24799=CARTESIAN_POINT('',(47.2724547499278,23.9648705799974,11.));
#24800=CARTESIAN_POINT('Origin',(47.3259909772385,25.1636757653237,11.));
#24801=CARTESIAN_POINT('',(47.9884049594373,22.4969551150606,11.));
#24802=CARTESIAN_POINT('Origin',(0.,0.,11.));
#24803=CARTESIAN_POINT('',(48.8290062914572,20.608933611151,11.));
#24804=CARTESIAN_POINT('Origin',(48.9660365296434,21.8010840688629,11.));
#24805=CARTESIAN_POINT('',(49.4408158756514,19.0946517525179,11.));
#24806=CARTESIAN_POINT('Origin',(0.,0.,11.));
#24807=CARTESIAN_POINT('',(50.1476678226092,17.1525919893539,11.));
#24808=CARTESIAN_POINT('Origin',(50.3675244741247,18.3322796822558,11.));
#24809=CARTESIAN_POINT('',(50.6523561066928,15.5993211660246,11.));
#24810=CARTESIAN_POINT('Origin',(0.,0.,11.));
#24811=CARTESIAN_POINT('',(51.2220149569554,13.6126846635571,11.));
#24812=CARTESIAN_POINT('Origin',(51.5236269022939,14.7741622717912,11.));
#24813=CARTESIAN_POINT('',(51.766094205967,11.3697621197168,11.));
#24814=CARTESIAN_POINT('Origin',(0.,0.,11.));
#24815=CARTESIAN_POINT('',(51.9151790989041,10.6683728435365,11.));
#24816=CARTESIAN_POINT('Origin',(52.428711399332,11.1440666278319,11.));
#24817=CARTESIAN_POINT('',(52.3304167585326,8.39806417445676,11.));
#24818=CARTESIAN_POINT('Origin',(0.,0.,11.));
#24819=CARTESIAN_POINT('',(52.6180453654948,6.35148029318636,11.));
#24820=CARTESIAN_POINT('Origin',(53.0783684845482,7.45967821145951,11.));
#24821=CARTESIAN_POINT('',(52.7887618365133,4.7272215695773,11.));
#24822=CARTESIAN_POINT('Origin',(0.,0.,11.));
#24823=CARTESIAN_POINT('',(52.9329273198661,2.66555910641112,11.));
#24824=CARTESIAN_POINT('Origin',(53.4694330939266,3.73894699268512,11.));
#24825=CARTESIAN_POINT('',(52.9987873134328,0.358529364921033,11.));
#24826=CARTESIAN_POINT('Origin',(0.,0.,11.));
#24827=CARTESIAN_POINT('',(52.9987873134328,-0.358529364921033,11.));
#24828=CARTESIAN_POINT('Origin',(53.6,0.,11.));
#24829=CARTESIAN_POINT('',(52.9329273198661,-2.66555910641113,11.));
#24830=CARTESIAN_POINT('Origin',(0.,0.,11.));
#24831=CARTESIAN_POINT('',(52.7887618365133,-4.72722156957733,11.));
#24832=CARTESIAN_POINT('Origin',(53.4694330939266,-3.73894699268513,11.));
#24833=CARTESIAN_POINT('',(52.6180453654948,-6.35148029318637,11.));
#24834=CARTESIAN_POINT('Origin',(0.,0.,11.));
#24835=CARTESIAN_POINT('',(52.3304167585326,-8.39806417445679,11.));
#24836=CARTESIAN_POINT('Origin',(53.0783684845482,-7.45967821145953,11.));
#24837=CARTESIAN_POINT('',(52.0468135832501,-10.0064577064218,11.));
#24838=CARTESIAN_POINT('Origin',(0.,0.,11.));
#24839=CARTESIAN_POINT('',(51.6171231503394,-12.0279922548487,11.));
#24840=CARTESIAN_POINT('Origin',(52.428711399332,-11.1440666278319,11.));
#24841=CARTESIAN_POINT('',(51.2220149569554,-13.6126846635571,11.));
#24842=CARTESIAN_POINT('Origin',(0.,0.,11.));
#24843=CARTESIAN_POINT('',(50.6523561066928,-15.5993211660246,11.));
#24844=CARTESIAN_POINT('Origin',(51.5236269022939,-14.7741622717911,11.));
#24845=CARTESIAN_POINT('',(50.1476678226092,-17.1525919893539,11.));
#24846=CARTESIAN_POINT('Origin',(0.,0.,11.));
#24847=CARTESIAN_POINT('',(49.4408158756514,-19.0946517525179,11.));
#24848=CARTESIAN_POINT('Origin',(50.3675244741247,-18.3322796822558,11.));
#24849=CARTESIAN_POINT('',(48.8290062914572,-20.608933611151,11.));
#24850=CARTESIAN_POINT('Origin',(0.,0.,11.));
#24851=CARTESIAN_POINT('',(47.9884049594373,-22.4969551150606,11.));
#24852=CARTESIAN_POINT('Origin',(48.9660365296434,-21.8010840688629,11.));
#24853=CARTESIAN_POINT('',(46.9634710240919,-24.5648608660681,11.));
#24854=CARTESIAN_POINT('Origin',(0.,0.,11.));
#24855=CARTESIAN_POINT('',(46.6268323415836,-25.1979861455206,11.));
#24856=CARTESIAN_POINT('Origin',(47.3259909772385,-25.1636757653237,11.));
#24857=CARTESIAN_POINT('',(45.4855965606673,-27.2040531083184,11.));
#24858=CARTESIAN_POINT('Origin',(0.,0.,11.));
#24859=CARTESIAN_POINT('',(44.390414095648,-28.9567114226892,11.));
#24860=CARTESIAN_POINT('Origin',(45.4553779539844,-28.4036725628998,11.));
#24861=CARTESIAN_POINT('',(43.4771371171594,-30.3107002244375,11.));
#24862=CARTESIAN_POINT('Origin',(0.,0.,11.));
#24863=CARTESIAN_POINT('',(42.2623631978924,-31.9826930843766,11.));
#24864=CARTESIAN_POINT('Origin',(43.3633108984972,-31.5052895228766,11.));
#24865=CARTESIAN_POINT('',(41.2568614319233,-33.2696766558841,11.));
#24866=CARTESIAN_POINT('Origin',(0.,0.,11.));
#24867=CARTESIAN_POINT('',(39.9284143148345,-34.8528582802461,11.));
#24868=CARTESIAN_POINT('Origin',(41.0599821511772,-34.4534158791985,11.));
#24869=CARTESIAN_POINT('',(38.3731925086332,-36.5581467896744,11.));
#24870=CARTESIAN_POINT('Origin',(0.,0.,11.));
#24871=CARTESIAN_POINT('',(37.8750816598376,-37.0739556732301,11.));
#24872=CARTESIAN_POINT('Origin',(38.5566132981517,-37.2336886566023,11.));
#24873=CARTESIAN_POINT('',(36.2251084243911,-38.6877437910394,11.));
#24874=CARTESIAN_POINT('Origin',(0.,0.,11.));
#24875=CARTESIAN_POINT('',(34.6892533672809,-40.0706338959167,11.));
#24876=CARTESIAN_POINT('Origin',(35.8654005008348,-39.8325626455884,11.));
#24877=CARTESIAN_POINT('',(33.4381452969578,-41.1204382162877,11.));
#24878=CARTESIAN_POINT('Origin',(0.,0.,11.));
#24879=CARTESIAN_POINT('',(31.809565968283,-42.3928238374073,11.));
#24880=CARTESIAN_POINT('Origin',(32.9994550774553,-42.2373763933203,11.));
#24881=CARTESIAN_POINT('',(30.4882748868283,-43.3527979999583,11.));
#24882=CARTESIAN_POINT('Origin',(0.,0.,11.));
#24883=CARTESIAN_POINT('',(28.774905561374,-44.5084802024738,11.));
#24884=CARTESIAN_POINT('Origin',(29.972739626032,-44.4364138889502,11.));
#24885=CARTESIAN_POINT('',(27.3898686661209,-45.3739473095812,11.));
#24886=CARTESIAN_POINT('Origin',(0.,0.,11.));
#24887=CARTESIAN_POINT('',(25.6000567070134,-46.4072957259707,11.));
#24888=CARTESIAN_POINT('Origin',(26.8,-46.4189616428459,11.));
#24889=CARTESIAN_POINT('',(24.1580217584921,-47.174039308885,11.));
#24890=CARTESIAN_POINT('Origin',(0.,0.,11.));
#24891=CARTESIAN_POINT('',(22.300486949685,-48.0800195695357,11.));
#24892=CARTESIAN_POINT('Origin',(23.4966934678945,-48.1753608816354,11.));
#24893=CARTESIAN_POINT('',(20.1861178092024,-49.0053124446014,11.));
#24894=CARTESIAN_POINT('Origin',(0.,0.,11.));
#24895=CARTESIAN_POINT('',(19.5212725321166,-49.2739273726667,11.));
#24896=CARTESIAN_POINT('Origin',(20.0789134070929,-49.6970546047798,11.));
#24897=CARTESIAN_POINT('',(17.3575602159692,-50.0770916023385,11.));
#24898=CARTESIAN_POINT('Origin',(0.,0.,11.));
#24899=CARTESIAN_POINT('',(15.3920147259482,-50.7157360458881,11.));
#24900=CARTESIAN_POINT('Origin',(16.5633108984972,-50.9766292734202,11.));
#24901=CARTESIAN_POINT('',(13.8220767461304,-51.1659085175284,11.));
#24902=CARTESIAN_POINT('Origin',(0.,0.,11.));
#24903=CARTESIAN_POINT('',(11.8167696417768,-51.6658877329441,11.));
#24904=CARTESIAN_POINT('Origin',(12.9670136041422,-52.0078509283934,11.));
#24905=CARTESIAN_POINT('',(10.2192535077747,-52.0054502696,11.));
#24906=CARTESIAN_POINT('Origin',(0.,0.,11.));
#24907=CARTESIAN_POINT('',(8.18395444372811,-52.3643284084021,11.));
#24908=CARTESIAN_POINT('Origin',(9.30754232294745,-52.7856955614544,11.));
#24909=CARTESIAN_POINT('',(6.56664309356483,-52.5916266955277,11.));
#24910=CARTESIAN_POINT('Origin',(0.,0.,11.));
#24911=CARTESIAN_POINT('',(4.51126784227785,-52.8076553394982,11.));
#24912=CARTESIAN_POINT('Origin',(5.6027256311462,-53.3063735917395,11.));
#24913=CARTESIAN_POINT('',(2.2079419616008,-52.953989389792,11.));
#24914=CARTESIAN_POINT('Origin',(0.,0.,11.));
#24915=CARTESIAN_POINT('',(1.49132004456263,-52.9790143785696,11.));
#24916=CARTESIAN_POINT('Origin',(1.87061302325407,-53.5673483282235,11.));
#24917=CARTESIAN_POINT('',(-0.816602797371066,-52.9937086819872,11.));
#24918=CARTESIAN_POINT('Origin',(0.,0.,11.));
#24919=CARTESIAN_POINT('',(-2.88204065427986,-52.9215820026866,11.));
#24920=CARTESIAN_POINT('Origin',(-1.87061302325404,-53.5673483282235,11.));
#24921=CARTESIAN_POINT('',(-4.51126784227786,-52.8076553394982,11.));
#24922=CARTESIAN_POINT('Origin',(0.,0.,11.));
#24923=CARTESIAN_POINT('',(-6.56664309356486,-52.5916266955277,11.));
#24924=CARTESIAN_POINT('Origin',(-5.60272563114622,-53.3063735917395,11.));
#24925=CARTESIAN_POINT('',(-8.18395444372813,-52.3643284084021,11.));
#24926=CARTESIAN_POINT('Origin',(0.,0.,11.));
#24927=CARTESIAN_POINT('',(-10.2192535077747,-52.0054502696,11.));
#24928=CARTESIAN_POINT('Origin',(-9.30754232294747,-52.7856955614544,11.));
#24929=CARTESIAN_POINT('',(-11.8167696417768,-51.6658877329441,11.));
#24930=CARTESIAN_POINT('Origin',(0.,0.,11.));
#24931=CARTESIAN_POINT('',(-13.8220767461304,-51.1659085175284,11.));
#24932=CARTESIAN_POINT('Origin',(-12.9670136041422,-52.0078509283934,11.));
#24933=CARTESIAN_POINT('',(-16.0365442723228,-50.5156336969243,11.));
#24934=CARTESIAN_POINT('Origin',(0.,0.,11.));
#24935=CARTESIAN_POINT('',(-16.7185076499055,-50.2940503634382,11.));
#24936=CARTESIAN_POINT('Origin',(-16.5633108984972,-50.9766292734202,11.));
#24937=CARTESIAN_POINT('',(-18.8922714615747,-49.5185023907445,11.));
#24938=CARTESIAN_POINT('Origin',(0.,0.,11.));
#24939=CARTESIAN_POINT('',(-20.8084793972118,-48.7443041305937,11.));
#24940=CARTESIAN_POINT('Origin',(-20.0789134070929,-49.6970546047798,11.));
#24941=CARTESIAN_POINT('',(-22.300486949685,-48.0800195695356,11.));
#24942=CARTESIAN_POINT('Origin',(0.,0.,11.));
#24943=CARTESIAN_POINT('',(-24.1580217584921,-47.1740393088849,11.));
#24944=CARTESIAN_POINT('Origin',(-23.4966934678946,-48.1753608816353,11.));
#24945=CARTESIAN_POINT('',(-25.6000567070134,-46.4072957259707,11.));
#24946=CARTESIAN_POINT('Origin',(0.,0.,11.));
#24947=CARTESIAN_POINT('',(-27.3898686661209,-45.3739473095812,11.));
#24948=CARTESIAN_POINT('Origin',(-26.8,-46.4189616428459,11.));
#24949=CARTESIAN_POINT('',(-28.774905561374,-44.5084802024739,11.));
#24950=CARTESIAN_POINT('Origin',(0.,0.,11.));
#24951=CARTESIAN_POINT('',(-30.4882748868283,-43.3527979999583,11.));
#24952=CARTESIAN_POINT('Origin',(-29.972739626032,-44.4364138889502,11.));
#24953=CARTESIAN_POINT('',(-31.809565968283,-42.3928238374073,11.));
#24954=CARTESIAN_POINT('Origin',(0.,0.,11.));
#24955=CARTESIAN_POINT('',(-33.4381452969578,-41.1204382162877,11.));
#24956=CARTESIAN_POINT('Origin',(-32.9994550774553,-42.2373763933203,11.));
#24957=CARTESIAN_POINT('',(-35.1966714489987,-39.6256775199017,11.));
#24958=CARTESIAN_POINT('Origin',(0.,0.,11.));
#24959=CARTESIAN_POINT('',(-35.7295499336443,-39.1458715772075,11.));
#24960=CARTESIAN_POINT('Origin',(-35.8654005008348,-39.8325626455883,11.));
#24961=CARTESIAN_POINT('',(-37.3999382108249,-37.5532238539713,11.));
#24962=CARTESIAN_POINT('Origin',(0.,0.,11.));
#24963=CARTESIAN_POINT('',(-38.835586464916,-36.0665665669195,11.));
#24964=CARTESIAN_POINT('Origin',(-38.5566132981517,-37.2336886566023,11.));
#24965=CARTESIAN_POINT('',(-39.9284143148345,-34.8528582802461,11.));
#24966=CARTESIAN_POINT('Origin',(0.,0.,11.));
#24967=CARTESIAN_POINT('',(-41.2568614319233,-33.2696766558841,11.));
#24968=CARTESIAN_POINT('Origin',(-41.0599821511772,-34.4534158791985,11.));
#24969=CARTESIAN_POINT('',(-42.2623631978924,-31.9826930843766,11.));
#24970=CARTESIAN_POINT('Origin',(0.,0.,11.));
#24971=CARTESIAN_POINT('',(-43.4771371171594,-30.3107002244375,11.));
#24972=CARTESIAN_POINT('Origin',(-43.3633108984972,-31.5052895228766,11.));
#24973=CARTESIAN_POINT('Origin',(0.,0.,11.));
#24974=CARTESIAN_POINT('',(-50.,6.12323399573677E-15,11.));
#24975=CARTESIAN_POINT('Origin',(0.,0.,11.));
#24976=CARTESIAN_POINT('Origin',(-51.5236269022939,-14.7741622717911,11.));
#24977=CARTESIAN_POINT('',(-50.8820099961117,-15.0540332165161,24.2));
#24978=CARTESIAN_POINT('',(-50.8820099961117,-15.0540332165161,14.5));
#24979=CARTESIAN_POINT('',(-51.1278139116532,-14.196813091104,24.2));
#24980=CARTESIAN_POINT('Origin',(-51.5236269022939,-14.7741622717911,24.2));
#24981=CARTESIAN_POINT('',(-51.1278139116532,-14.196813091104,11.0622545443405));
#24982=CARTESIAN_POINT('',(-51.1278139116532,-14.196813091104,14.5));
#24983=CARTESIAN_POINT('Ctrl Pts',(-51.0445282617143,-14.2638050512144,
11.));
#24984=CARTESIAN_POINT('Ctrl Pts',(-51.0716596511096,-14.2383354169029,
11.0192757561174));
#24985=CARTESIAN_POINT('Ctrl Pts',(-51.0998585632662,-14.2159784253933,
11.0404460254343));
#24986=CARTESIAN_POINT('Ctrl Pts',(-51.1278139116532,-14.196813091104,11.0622545443405));
#24987=CARTESIAN_POINT('Origin',(-50.9840802240917,-15.4714365365519,14.5));
#24988=CARTESIAN_POINT('',(-51.0861504520717,-15.8888398565878,24.2));
#24989=CARTESIAN_POINT('',(-51.0861504520717,-15.8888398565878,14.5));
#24990=CARTESIAN_POINT('',(-50.9188578780728,-15.204717981028,24.2));
#24991=CARTESIAN_POINT('Origin',(-37.7528714186306,-37.5960434680236,14.5));
#24992=CARTESIAN_POINT('',(-37.7445797725392,-37.6286709684663,11.2969997378715));
#24993=CARTESIAN_POINT('',(-37.6470350917589,-38.0125077941442,11.5));
#24994=CARTESIAN_POINT('Ctrl Pts',(-37.7445797725392,-37.6286709684663,
11.2969997378715));
#24995=CARTESIAN_POINT('Ctrl Pts',(-37.6959001388536,-37.8202245818423,
11.3977655520827));
#24996=CARTESIAN_POINT('Ctrl Pts',(-37.6470350917589,-38.0125077941442,
11.5));
#24997=CARTESIAN_POINT('',(-37.6470350917589,-38.0125077941442,24.2));
#24998=CARTESIAN_POINT('',(-37.6470350917589,-38.0125077941442,14.5));
#24999=CARTESIAN_POINT('',(-37.8587077455022,-37.179579141903,24.2));
#25000=CARTESIAN_POINT('',(-37.8205002822983,-37.329924924739,24.2));
#25001=CARTESIAN_POINT('',(-37.8587077455022,-37.179579141903,11.5));
#25002=CARTESIAN_POINT('',(-37.8587077455022,-37.179579141903,14.5));
#25003=CARTESIAN_POINT('Ctrl Pts',(-37.8587077455022,-37.179579141903,11.5));
#25004=CARTESIAN_POINT('Ctrl Pts',(-37.8088702108732,-37.3756890777659,
11.4654707447276));
#25005=CARTESIAN_POINT('Ctrl Pts',(-37.7445797725392,-37.6286709684663,
11.2969997378715));
#25006=CARTESIAN_POINT('Origin',(-38.5566132981517,-37.2336886566023,11.25));
#25007=CARTESIAN_POINT('',(-38.4781801929734,-36.5380966439885,11.5));
#25008=CARTESIAN_POINT('Origin',(-38.5566132981517,-37.2336886566023,11.5));
#25009=CARTESIAN_POINT('',(-38.923015436114,-36.4083651159828,11.2969997378716));
#25010=CARTESIAN_POINT('Ctrl Pts',(-38.923015436114,-36.4083651159828,11.2969997378716));
#25011=CARTESIAN_POINT('Ctrl Pts',(-38.6724313590868,-36.4814453309791,
11.4654707447277));
#25012=CARTESIAN_POINT('Ctrl Pts',(-38.4781801929734,-36.5380966439885,
11.5));
#25013=CARTESIAN_POINT('Ctrl Pts',(-38.923015436114,-36.4083651159828,11.2969997378716));
#25014=CARTESIAN_POINT('Ctrl Pts',(-38.8990006050577,-36.2901863355678,
11.1987310576087));
#25015=CARTESIAN_POINT('Ctrl Pts',(-38.868187176743,-36.1742932195071,11.0971961933879));
#25016=CARTESIAN_POINT('Ctrl Pts',(-38.835586464916,-36.0665665669195,11.));
#25017=CARTESIAN_POINT('Ctrl Pts',(-37.7445797725392,-37.6286709684663,
11.2969997378715));
#25018=CARTESIAN_POINT('Ctrl Pts',(-37.6256348779269,-37.6087951465537,
11.1987310576087));
#25019=CARTESIAN_POINT('Ctrl Pts',(-37.5087369876815,-37.5820451003687,
11.0971961933879));
#25020=CARTESIAN_POINT('Ctrl Pts',(-37.399938210825,-37.5532238539713,11.));
#25021=CARTESIAN_POINT('Origin',(-38.5566132981517,-37.2336886566023,11.));
#25022=CARTESIAN_POINT('',(-38.4781801929734,-36.5380966439885,24.2));
#25023=CARTESIAN_POINT('Origin',(-38.5566132981517,-37.2336886566023,24.2));
#25024=CARTESIAN_POINT('',(-38.4781801929734,-36.5380966439885,14.5));
#25025=CARTESIAN_POINT('Origin',(-38.8906971857383,-36.4177903943715,14.5));
#25026=CARTESIAN_POINT('',(-39.3032141785032,-36.2974841447544,24.2));
#25027=CARTESIAN_POINT('',(-38.6271009679847,-36.4946654635865,24.2));
#25028=CARTESIAN_POINT('',(-39.3032141785032,-36.2974841447544,11.5));
#25029=CARTESIAN_POINT('',(-39.3032141785032,-36.2974841447545,14.5));
#25030=CARTESIAN_POINT('Ctrl Pts',(-39.3032141785032,-36.2974841447544,
11.5));
#25031=CARTESIAN_POINT('Ctrl Pts',(-39.1127534654889,-36.3530300119163,
11.3977655520827));
#25032=CARTESIAN_POINT('Ctrl Pts',(-38.923015436114,-36.4083651159828,11.2969997378716));
#25033=CARTESIAN_POINT('Origin',(-40.2834747403675,-34.8709542118271,14.5));
#25034=CARTESIAN_POINT('',(-40.2774792716873,-34.9040806293113,11.2969997378715));
#25035=CARTESIAN_POINT('',(-40.2069473082991,-35.2937868207374,11.5));
#25036=CARTESIAN_POINT('Ctrl Pts',(-40.2774792716873,-34.9040806293113,
11.2969997378715));
#25037=CARTESIAN_POINT('Ctrl Pts',(-40.2422803237447,-35.0985633473019,
11.3977655520827));
#25038=CARTESIAN_POINT('Ctrl Pts',(-40.2069473082991,-35.2937868207374,
11.5));
#25039=CARTESIAN_POINT('',(-40.2069473082991,-35.2937868207374,24.2));
#25040=CARTESIAN_POINT('',(-40.2069473082991,-35.2937868207374,14.5));
#25041=CARTESIAN_POINT('',(-40.3600021724359,-34.4481216029168,24.2));
#25042=CARTESIAN_POINT('',(-40.332375372345,-34.600766368886,24.2));
#25043=CARTESIAN_POINT('',(-40.3600021724359,-34.4481216029168,11.5));
#25044=CARTESIAN_POINT('',(-40.3600021724359,-34.4481216029168,14.5));
#25045=CARTESIAN_POINT('Ctrl Pts',(-40.3600021724359,-34.4481216029168,
11.5));
#25046=CARTESIAN_POINT('Ctrl Pts',(-40.3239659771285,-34.6472303155083,
11.4654707447276));
#25047=CARTESIAN_POINT('Ctrl Pts',(-40.2774792716873,-34.9040806293113,
11.2969997378715));
#25048=CARTESIAN_POINT('Origin',(-41.0599821511772,-34.4534158791985,11.25));
#25049=CARTESIAN_POINT('',(-40.9332180591367,-33.7649895106091,11.5));
#25050=CARTESIAN_POINT('Origin',(-41.0599821511772,-34.4534158791985,11.5));
#25051=CARTESIAN_POINT('',(-41.3679200920551,-33.6045438641267,11.2969997378715));
#25052=CARTESIAN_POINT('Ctrl Pts',(-41.3679200920551,-33.6045438641267,
11.2969997378715));
#25053=CARTESIAN_POINT('Ctrl Pts',(-41.1230442433439,-33.6949259209821,
11.4654707447276));
#25054=CARTESIAN_POINT('Ctrl Pts',(-40.9332180591367,-33.7649895106091,
11.5));
#25055=CARTESIAN_POINT('Ctrl Pts',(-41.3679200920551,-33.6045438641267,
11.2969997378715));
#25056=CARTESIAN_POINT('Ctrl Pts',(-41.3357200249272,-33.4883281512132,
11.1987310576086));
#25057=CARTESIAN_POINT('Ctrl Pts',(-41.2968973614675,-33.3748667810618,
11.0971961933879));
#25058=CARTESIAN_POINT('Ctrl Pts',(-41.2568614319233,-33.2696766558841,
11.));
#25059=CARTESIAN_POINT('Ctrl Pts',(-40.2774792716873,-34.9040806293113,
11.2969997378715));
#25060=CARTESIAN_POINT('Ctrl Pts',(-40.1574376536108,-34.8925504003199,
11.1987310576086));
#25061=CARTESIAN_POINT('Ctrl Pts',(-40.0389585318563,-34.8740199005147,
11.0971961933879));
#25062=CARTESIAN_POINT('Ctrl Pts',(-39.9284143148345,-34.8528582802461,
11.));
#25063=CARTESIAN_POINT('Origin',(-41.0599821511772,-34.4534158791985,11.));
#25064=CARTESIAN_POINT('',(-40.9332180591367,-33.7649895106091,24.2));
#25065=CARTESIAN_POINT('Origin',(-41.0599821511772,-34.4534158791985,24.2));
#25066=CARTESIAN_POINT('',(-40.9332180591367,-33.7649895106091,14.5));
#25067=CARTESIAN_POINT('Origin',(-41.3363380414977,-33.6162005901946,14.5));
#25068=CARTESIAN_POINT('',(-41.7394580238587,-33.4674116697801,24.2));
#25069=CARTESIAN_POINT('',(-41.0787464646293,-33.7112759382477,24.2));
#25070=CARTESIAN_POINT('',(-41.7394580238587,-33.4674116697801,11.5));
#25071=CARTESIAN_POINT('',(-41.7394580238587,-33.4674116697801,14.5));
#25072=CARTESIAN_POINT('Ctrl Pts',(-41.7394580238587,-33.4674116697801,
11.5));
#25073=CARTESIAN_POINT('Ctrl Pts',(-41.5533359473925,-33.5361080977283,
11.3977655520824));
#25074=CARTESIAN_POINT('Ctrl Pts',(-41.3679200920551,-33.6045438641267,
11.2969997378715));
#25075=CARTESIAN_POINT('Origin',(-42.6178210224503,-31.9759771719266,14.5));
#25076=CARTESIAN_POINT('',(-42.6141509405019,-32.0094411178763,11.2969997378715));
#25077=CARTESIAN_POINT('',(-42.5709753191418,-32.4031180656588,11.5));
#25078=CARTESIAN_POINT('Ctrl Pts',(-42.6141509405019,-32.0094411178763,
11.2969997378715));
#25079=CARTESIAN_POINT('Ctrl Pts',(-42.5926041640386,-32.2059054402279,
11.3977655520824));
#25080=CARTESIAN_POINT('Ctrl Pts',(-42.5709753191418,-32.4031180656588,
11.5));
#25081=CARTESIAN_POINT('',(-42.5709753191418,-32.4031180656588,24.2));
#25082=CARTESIAN_POINT('',(-42.5709753191418,-32.4031180656588,14.5));
#25083=CARTESIAN_POINT('',(-42.6646667257588,-31.5488362781943,24.2));
#25084=CARTESIAN_POINT('',(-42.6477551837739,-31.7030363573407,24.2));
#25085=CARTESIAN_POINT('',(-42.6646667257588,-31.5488362781943,11.5));
#25086=CARTESIAN_POINT('',(-42.6646667257588,-31.5488362781943,14.5));
#25087=CARTESIAN_POINT('Ctrl Pts',(-42.6646667257588,-31.5488362781943,
11.5));
#25088=CARTESIAN_POINT('Ctrl Pts',(-42.642607434494,-31.7499737298808,11.4654707447276));
#25089=CARTESIAN_POINT('Ctrl Pts',(-42.6141509405019,-32.0094411178763,
11.2969997378715));
#25090=CARTESIAN_POINT('Origin',(-43.3633108984972,-31.5052895228766,11.25));
#25091=CARTESIAN_POINT('',(-43.1888334015084,-30.827382742379,11.5));
#25092=CARTESIAN_POINT('Origin',(-43.3633108984972,-31.5052895228766,11.5));
#25093=CARTESIAN_POINT('',(-43.6112843995965,-30.6370046524817,11.2969997378715));
#25094=CARTESIAN_POINT('Ctrl Pts',(-43.6112843995965,-30.6370046524817,
11.2969997378715));
#25095=CARTESIAN_POINT('Ctrl Pts',(-43.3733097897213,-30.7442482189004,
11.4654707447276));
#25096=CARTESIAN_POINT('Ctrl Pts',(-43.1888334015084,-30.827382742379,11.5));
#25097=CARTESIAN_POINT('Ctrl Pts',(-43.6112843995965,-30.6370046524817,
11.2969997378715));
#25098=CARTESIAN_POINT('Ctrl Pts',(-43.5710559718872,-30.523318198341,11.1987310576087));
#25099=CARTESIAN_POINT('Ctrl Pts',(-43.5244132133966,-30.412841346489,11.0971961933879));
#25100=CARTESIAN_POINT('Ctrl Pts',(-43.4771371171594,-30.3107002244375,
11.));
#25101=CARTESIAN_POINT('Ctrl Pts',(-42.6141509405019,-32.0094411178763,
11.2969997378715));
#25102=CARTESIAN_POINT('Ctrl Pts',(-42.4935974296578,-32.0063126559227,
11.1987310576086));
#25103=CARTESIAN_POINT('Ctrl Pts',(-42.3741142947661,-31.9960919812296,
11.0971961933879));
#25104=CARTESIAN_POINT('Ctrl Pts',(-42.2623631978924,-31.9826930843766,
11.));
#25105=CARTESIAN_POINT('Origin',(-43.3633108984972,-31.5052895228766,11.));
#25106=CARTESIAN_POINT('',(-43.1888334015084,-30.827382742379,24.2));
#25107=CARTESIAN_POINT('Origin',(-43.3633108984972,-31.5052895228766,24.2));
#25108=CARTESIAN_POINT('',(-43.1888334015084,-30.827382742379,14.5));
#25109=CARTESIAN_POINT('Origin',(-44.74453756444,-28.9252163854583,14.5));
#25110=CARTESIAN_POINT('',(-44.727601817449,-29.3545845765143,11.5));
#25111=CARTESIAN_POINT('Ctrl Pts',(-44.7614733114311,-28.4958481944022,
11.0622545443403));
#25112=CARTESIAN_POINT('Ctrl Pts',(-44.744607134536,-28.9234525904335,11.2776618075214));
#25113=CARTESIAN_POINT('Ctrl Pts',(-44.727601817449,-29.3545845765143,11.5));
#25114=CARTESIAN_POINT('',(-44.727601817449,-29.3545845765143,24.2));
#25115=CARTESIAN_POINT('',(-44.727601817449,-29.3545845765143,14.5));
#25116=CARTESIAN_POINT('',(-44.7553594188848,-28.6508523394404,24.2));
#25117=CARTESIAN_POINT('Origin',(0.,0.,14.5));
#25118=CARTESIAN_POINT('',(-43.9723514253571,-30.4742893292837,11.5));
#25119=CARTESIAN_POINT('Origin',(0.,0.,11.5));
#25120=CARTESIAN_POINT('',(-43.9723514253571,-30.4742893292837,24.2));
#25121=CARTESIAN_POINT('',(-43.9723514253571,-30.4742893292837,14.5));
#25122=CARTESIAN_POINT('Origin',(0.,0.,24.2));
#25123=CARTESIAN_POINT('Origin',(0.,0.,11.25));
#25124=CARTESIAN_POINT('Ctrl Pts',(-43.9723514253571,-30.4742893292837,
11.5));
#25125=CARTESIAN_POINT('Ctrl Pts',(-43.7914747534877,-30.555801635926,11.3977655520827));
#25126=CARTESIAN_POINT('Ctrl Pts',(-43.6112843995965,-30.6370046524817,
11.2969997378715));
#25127=CARTESIAN_POINT('Origin',(-43.5805924134327,-30.6508360358314,14.5));
#25128=CARTESIAN_POINT('',(-43.3302604377194,-30.7636484651835,24.2));
#25129=CARTESIAN_POINT('Origin',(-17.2413304950988,-50.4130767515726,14.5));
#25130=CARTESIAN_POINT('',(-17.6620417438948,-50.5005176353364,24.2));
#25131=CARTESIAN_POINT('',(-16.8206192463028,-50.3256358678088,24.2));
#25132=CARTESIAN_POINT('',(-16.9724981902626,-50.3572024805936,24.2));
#25133=CARTESIAN_POINT('',(-17.6620417438948,-50.5005176353364,11.5));
#25134=CARTESIAN_POINT('',(-17.6620417438948,-50.5005176353364,14.5));
#25135=CARTESIAN_POINT('',(-16.8206192463027,-50.3256358678088,11.0622545443403));
#25136=CARTESIAN_POINT('Ctrl Pts',(-17.6620417438948,-50.5005176353364,
11.5));
#25137=CARTESIAN_POINT('Ctrl Pts',(-17.2396022617919,-50.412717554503,11.27766180752));
#25138=CARTESIAN_POINT('Ctrl Pts',(-16.8206192463027,-50.3256358678088,
11.0622545443403));
#25139=CARTESIAN_POINT('',(-16.8206192463028,-50.3256358678088,14.5));
#25140=CARTESIAN_POINT('Origin',(0.,0.,11.25));
#25141=CARTESIAN_POINT('',(-18.9311980867048,-50.0385825039234,11.5));
#25142=CARTESIAN_POINT('Origin',(0.,0.,11.5));
#25143=CARTESIAN_POINT('',(-19.1764300887141,-49.7276051113597,11.2969997378715));
#25144=CARTESIAN_POINT('Ctrl Pts',(-19.1764300887141,-49.7276051113597,
11.2969997378715));
#25145=CARTESIAN_POINT('Ctrl Pts',(-19.0540471568067,-49.8827982539636,
11.3977655520831));
#25146=CARTESIAN_POINT('Ctrl Pts',(-18.9311980867048,-50.0385825039234,
11.5));
#25147=CARTESIAN_POINT('Ctrl Pts',(-19.1764300887141,-49.7276051113597,
11.2969997378715));
#25148=CARTESIAN_POINT('Ctrl Pts',(-19.0758527456145,-49.6610683973889,
11.1987310576087));
#25149=CARTESIAN_POINT('Ctrl Pts',(-18.9799414329601,-49.5890843587438,
11.0971961933879));
#25150=CARTESIAN_POINT('Ctrl Pts',(-18.8922714615747,-49.5185023907445,
11.));
#25151=CARTESIAN_POINT('Ctrl Pts',(-16.8206192463027,-50.3256358678088,
11.0622545443403));
#25152=CARTESIAN_POINT('Ctrl Pts',(-16.7890977128585,-50.3131768265636,
11.0404458048696));
#25153=CARTESIAN_POINT('Ctrl Pts',(-16.7547950072711,-50.3023009552715,
11.0192759649605));
#25154=CARTESIAN_POINT('Ctrl Pts',(-16.7185076499055,-50.2940503634382,
11.));
#25155=CARTESIAN_POINT('Origin',(0.,0.,14.5));
#25156=CARTESIAN_POINT('',(-18.9311980867048,-50.0385825039234,24.2));
#25157=CARTESIAN_POINT('Origin',(0.,0.,24.2));
#25158=CARTESIAN_POINT('',(-18.9311980867048,-50.0385825039234,14.5));
#25159=CARTESIAN_POINT('Origin',(-19.1972756843392,-49.7011709228329,14.5));
#25160=CARTESIAN_POINT('',(-19.4633532819736,-49.3637593417425,24.2));
#25161=CARTESIAN_POINT('',(-19.3672978885043,-49.485566673404,24.2));
#25162=CARTESIAN_POINT('',(-19.4633532819736,-49.3637593417425,11.5));
#25163=CARTESIAN_POINT('',(-19.4633532819736,-49.3637593417425,14.5));
#25164=CARTESIAN_POINT('Ctrl Pts',(-19.4633532819736,-49.3637593417425,
11.5));
#25165=CARTESIAN_POINT('Ctrl Pts',(-19.3380593316065,-49.5226439313144,
11.4654707447276));
#25166=CARTESIAN_POINT('Ctrl Pts',(-19.1764300887141,-49.7276051113597,
11.2969997378715));
#25167=CARTESIAN_POINT('Origin',(-20.7159699453405,-49.087578612363,14.5));
#25168=CARTESIAN_POINT('',(-21.1417559303916,-49.1454591613483,24.2));
#25169=CARTESIAN_POINT('',(-20.2901839602894,-49.0296980633778,24.2));
#25170=CARTESIAN_POINT('',(-20.4438949103711,-49.0505932419138,24.2));
#25171=CARTESIAN_POINT('',(-21.1417559303916,-49.1454591613483,11.5));
#25172=CARTESIAN_POINT('',(-21.1417559303916,-49.1454591613483,14.5));
#25173=CARTESIAN_POINT('',(-20.7493277422619,-49.0921132087719,11.2969997378715));
#25174=CARTESIAN_POINT('Ctrl Pts',(-21.1417559303916,-49.1454591613483,
11.5));
#25175=CARTESIAN_POINT('Ctrl Pts',(-20.945168871612,-49.1187354849356,11.3977655520828));
#25176=CARTESIAN_POINT('Ctrl Pts',(-20.7493277422619,-49.0921132087719,
11.2969997378715));
#25177=CARTESIAN_POINT('',(-20.2901839602894,-49.0296980633778,11.5));
#25178=CARTESIAN_POINT('Ctrl Pts',(-20.7493277422619,-49.0921132087719,
11.2969997378715));
#25179=CARTESIAN_POINT('Ctrl Pts',(-20.4906833956133,-49.056953580927,11.4654707447276));
#25180=CARTESIAN_POINT('Ctrl Pts',(-20.2901839602894,-49.0296980633778,
11.5));
#25181=CARTESIAN_POINT('',(-20.2901839602894,-49.0296980633778,14.5));
#25182=CARTESIAN_POINT('Origin',(0.,0.,11.25));
#25183=CARTESIAN_POINT('',(-22.3755977062724,-48.5961174095941,11.5));
#25184=CARTESIAN_POINT('Origin',(0.,0.,11.5));
#25185=CARTESIAN_POINT('',(-22.5985396491308,-48.2687910226197,11.2969997378715));
#25186=CARTESIAN_POINT('Ctrl Pts',(-22.5985396491308,-48.2687910226197,
11.2969997378715));
#25187=CARTESIAN_POINT('Ctrl Pts',(-22.4872805622725,-48.4321431243036,
11.3977655520825));
#25188=CARTESIAN_POINT('Ctrl Pts',(-22.3755977062724,-48.5961174095941,
11.5));
#25189=CARTESIAN_POINT('Ctrl Pts',(-22.5985396491308,-48.2687910226197,
11.2969997378715));
#25190=CARTESIAN_POINT('Ctrl Pts',(-22.4935659408428,-48.2094323095332,
11.1987310576086));
#25191=CARTESIAN_POINT('Ctrl Pts',(-22.3928669106239,-48.1443140553513,
11.0971961933879));
#25192=CARTESIAN_POINT('Ctrl Pts',(-22.300486949685,-48.0800195695356,11.));
#25193=CARTESIAN_POINT('Ctrl Pts',(-20.7493277422619,-49.0921132087719,
11.2969997378715));
#25194=CARTESIAN_POINT('Ctrl Pts',(-20.7754567428632,-48.9743838089662,
11.1987310576087));
#25195=CARTESIAN_POINT('Ctrl Pts',(-20.7944452523739,-48.8559772288226,
11.0971961933879));
#25196=CARTESIAN_POINT('Ctrl Pts',(-20.8084793972118,-48.7443041305937,
11.));
#25197=CARTESIAN_POINT('Origin',(0.,0.,14.5));
#25198=CARTESIAN_POINT('',(-22.3755977062724,-48.5961174095941,24.2));
#25199=CARTESIAN_POINT('Origin',(0.,0.,24.2));
#25200=CARTESIAN_POINT('',(-22.3755977062724,-48.5961174095941,14.5));
#25201=CARTESIAN_POINT('Origin',(-22.6174905101547,-48.2409671112037,14.5));
#25202=CARTESIAN_POINT('',(-22.859383314037,-47.8858168128132,24.2));
#25203=CARTESIAN_POINT('',(-22.7720587566113,-48.0140279134694,24.2));
#25204=CARTESIAN_POINT('',(-22.859383314037,-47.8858168128132,11.5));
#25205=CARTESIAN_POINT('',(-22.859383314037,-47.8858168128132,14.5));
#25206=CARTESIAN_POINT('Ctrl Pts',(-22.859383314037,-47.8858168128132,11.5));
#25207=CARTESIAN_POINT('Ctrl Pts',(-22.7454778021365,-48.0530544316696,
11.4654707447276));
#25208=CARTESIAN_POINT('Ctrl Pts',(-22.5985396491308,-48.2687910226197,
11.2969997378715));
#25209=CARTESIAN_POINT('Origin',(-24.0896832723708,-47.5229307244201,14.5));
#25210=CARTESIAN_POINT('',(-24.5184696071579,-47.5509689504102,24.2));
#25211=CARTESIAN_POINT('',(-23.6608969375837,-47.49489249843,24.2));
#25212=CARTESIAN_POINT('',(-23.8156910294893,-47.5050144435077,24.2));
#25213=CARTESIAN_POINT('',(-24.5184696071579,-47.5509689504102,11.5));
#25214=CARTESIAN_POINT('',(-24.5184696071579,-47.5509689504102,14.5));
#25215=CARTESIAN_POINT('',(-24.1232761288307,-47.5251273524949,11.2969997378715));
#25216=CARTESIAN_POINT('Ctrl Pts',(-24.5184696071579,-47.5509689504102,
11.5));
#25217=CARTESIAN_POINT('Ctrl Pts',(-24.3204972751409,-47.5380235915343,
11.3977655520827));
#25218=CARTESIAN_POINT('Ctrl Pts',(-24.1232761288307,-47.5251273524949,
11.2969997378715));
#25219=CARTESIAN_POINT('',(-23.6608969375837,-47.49489249843,11.5));
#25220=CARTESIAN_POINT('Ctrl Pts',(-24.1232761288307,-47.5251273524949,
11.2969997378715));
#25221=CARTESIAN_POINT('Ctrl Pts',(-23.8628092151545,-47.5080954893125,
11.4654707447276));
#25222=CARTESIAN_POINT('Ctrl Pts',(-23.6608969375837,-47.49489249843,11.5));
#25223=CARTESIAN_POINT('',(-23.6608969375837,-47.49489249843,14.5));
#25224=CARTESIAN_POINT('Origin',(0.,0.,11.25));
#25225=CARTESIAN_POINT('',(-25.7109856630024,-46.9168969161099,11.5));
#25226=CARTESIAN_POINT('Origin',(0.,0.,11.5));
#25227=CARTESIAN_POINT('',(-25.9105513959742,-46.5748162359794,11.2969997378715));
#25228=CARTESIAN_POINT('Ctrl Pts',(-25.9105513959742,-46.5748162359794,
11.2969997378715));
#25229=CARTESIAN_POINT('Ctrl Pts',(-25.8109581972506,-46.7455314617269,
11.3977655520837));
#25230=CARTESIAN_POINT('Ctrl Pts',(-25.7109856630024,-46.9168969161099,
11.5));
#25231=CARTESIAN_POINT('Ctrl Pts',(-25.9105513959742,-46.5748162359794,
11.2969997378714));
#25232=CARTESIAN_POINT('Ctrl Pts',(-25.8016927438527,-46.5229247134606,
11.1987310576086));
#25233=CARTESIAN_POINT('Ctrl Pts',(-25.6966965916221,-46.4649894933305,
11.0971961933879));
#25234=CARTESIAN_POINT('Ctrl Pts',(-25.6000567070135,-46.4072957259707,
11.));
#25235=CARTESIAN_POINT('Ctrl Pts',(-24.1232761288307,-47.5251273524949,
11.2969997378715));
#25236=CARTESIAN_POINT('Ctrl Pts',(-24.1411290927132,-47.4058620686457,
11.1987310576086));
#25237=CARTESIAN_POINT('Ctrl Pts',(-24.1518117216703,-47.2864193495151,
11.0971961933879));
#25238=CARTESIAN_POINT('Ctrl Pts',(-24.1580217584921,-47.174039308885,11.));
#25239=CARTESIAN_POINT('Origin',(0.,0.,14.5));
#25240=CARTESIAN_POINT('',(-25.7109856630024,-46.9168969161099,24.2));
#25241=CARTESIAN_POINT('Origin',(0.,0.,24.2));
#25242=CARTESIAN_POINT('',(-25.7109856630024,-46.9168969161099,14.5));
#25243=CARTESIAN_POINT('Origin',(-25.927515195707,-46.5457381569737,14.5));
#25244=CARTESIAN_POINT('',(-26.1440447284116,-46.1745793978374,24.2));
#25245=CARTESIAN_POINT('',(-26.0658764434955,-46.3085696358935,24.2));
#25246=CARTESIAN_POINT('',(-26.1440447284116,-46.1745793978374,11.5));
#25247=CARTESIAN_POINT('',(-26.1440447284116,-46.1745793978374,14.5));
#25248=CARTESIAN_POINT('Ctrl Pts',(-26.1440447284116,-46.1745793978374,
11.5));
#25249=CARTESIAN_POINT('Ctrl Pts',(-26.0420825911821,-46.3493552811098,
11.4654707447276));
#25250=CARTESIAN_POINT('Ctrl Pts',(-25.9105513959742,-46.5748162359794,
11.2969997378715));
#25251=CARTESIAN_POINT('Origin',(-27.3460340839844,-45.7267558949761,14.5));
#25252=CARTESIAN_POINT('',(-27.7757317645859,-45.7248151985525,24.2));
#25253=CARTESIAN_POINT('',(-26.916336403383,-45.7286965913998,24.2));
#25254=CARTESIAN_POINT('',(-27.0714594958568,-45.7279959899202,24.2));
#25255=CARTESIAN_POINT('',(-27.7757317645859,-45.7248151985525,11.5));
#25256=CARTESIAN_POINT('',(-27.7757317645859,-45.7248151985525,14.5));
#25257=CARTESIAN_POINT('',(-27.379698338963,-45.7266038529657,11.2969997378715));
#25258=CARTESIAN_POINT('Ctrl Pts',(-27.7757317645859,-45.7248151985525,
11.5));
#25259=CARTESIAN_POINT('Ctrl Pts',(-27.5773386606333,-45.7257112257006,
11.3977655520828));
#25260=CARTESIAN_POINT('Ctrl Pts',(-27.379698338963,-45.7266038529657,11.2969997378715));
#25261=CARTESIAN_POINT('',(-26.916336403383,-45.7286965913998,11.5));
#25262=CARTESIAN_POINT('Ctrl Pts',(-27.379698338963,-45.7266038529657,11.2969997378715));
#25263=CARTESIAN_POINT('Ctrl Pts',(-27.1186778268806,-45.727782731971,11.4654707447276));
#25264=CARTESIAN_POINT('Ctrl Pts',(-26.916336403383,-45.7286965913998,11.5));
#25265=CARTESIAN_POINT('',(-26.916336403383,-45.7286965913998,14.5));
#25266=CARTESIAN_POINT('Origin',(0.,0.,11.25));
#25267=CARTESIAN_POINT('',(-28.9211122820413,-45.0091020169205,11.5));
#25268=CARTESIAN_POINT('Origin',(0.,0.,11.5));
#25269=CARTESIAN_POINT('',(-29.0963295409359,-44.6539336263215,11.2969997378715));
#25270=CARTESIAN_POINT('Ctrl Pts',(-29.0963295409359,-44.6539336263215,
11.2969997378715));
#25271=CARTESIAN_POINT('Ctrl Pts',(-29.0088874384024,-44.8311802687092,
11.3977655520826));
#25272=CARTESIAN_POINT('Ctrl Pts',(-28.9211122820413,-45.0091020169205,
11.5));
#25273=CARTESIAN_POINT('Ctrl Pts',(-29.0963295409359,-44.6539336263215,
11.2969997378715));
#25274=CARTESIAN_POINT('Ctrl Pts',(-28.9841162933917,-44.6097621046521,
11.1987310576087));
#25275=CARTESIAN_POINT('Ctrl Pts',(-28.875334549849,-44.5592921731428,11.0971961933879));
#25276=CARTESIAN_POINT('Ctrl Pts',(-28.774905561374,-44.5084802024738,11.));
#25277=CARTESIAN_POINT('Ctrl Pts',(-27.379698338963,-45.7266038529657,11.2969997378715));
#25278=CARTESIAN_POINT('Ctrl Pts',(-27.3891882882814,-45.6063837335473,
11.1987310576086));
#25279=CARTESIAN_POINT('Ctrl Pts',(-27.3915129919902,-45.486486788351,11.0971961933879));
#25280=CARTESIAN_POINT('Ctrl Pts',(-27.3898686661209,-45.3739473095812,
11.));
#25281=CARTESIAN_POINT('Origin',(0.,0.,14.5));
#25282=CARTESIAN_POINT('',(-28.9211122820413,-45.0091020169205,24.2));
#25283=CARTESIAN_POINT('Origin',(0.,0.,24.2));
#25284=CARTESIAN_POINT('',(-28.9211122820413,-45.0091020169205,14.5));
#25285=CARTESIAN_POINT('Origin',(-29.1112236334504,-44.6237430452042,14.5));
#25286=CARTESIAN_POINT('',(-29.3013349848595,-44.2383840734879,24.2));
#25287=CARTESIAN_POINT('',(-29.2327038004797,-44.3775006619728,24.2));
#25288=CARTESIAN_POINT('',(-29.3013349848595,-44.2383840734879,11.5));
#25289=CARTESIAN_POINT('',(-29.3013349848595,-44.2383840734879,14.5));
#25290=CARTESIAN_POINT('Ctrl Pts',(-29.3013349848595,-44.2383840734879,
11.5));
#25291=CARTESIAN_POINT('Ctrl Pts',(-29.2118129715843,-44.4198467306414,
11.4654707447275));
#25292=CARTESIAN_POINT('Ctrl Pts',(-29.0963295409359,-44.6539336263215,
11.2969997378715));
#25293=CARTESIAN_POINT('Origin',(-30.4691577663544,-43.7078049072494,14.5));
#25294=CARTESIAN_POINT('',(-30.8976733488633,-43.67589474329,24.2));
#25295=CARTESIAN_POINT('',(-30.0406421838456,-43.7397150712088,24.2));
#25296=CARTESIAN_POINT('',(-30.1953385327739,-43.728195336432,24.2));
#25297=CARTESIAN_POINT('',(-30.8976733488633,-43.67589474329,11.5));
#25298=CARTESIAN_POINT('',(-30.8976733488632,-43.67589474329,14.5));
#25299=CARTESIAN_POINT('',(-30.5027294109855,-43.7053049358871,11.2969997378715));
#25300=CARTESIAN_POINT('Ctrl Pts',(-30.8976733488633,-43.67589474329,11.5));
#25301=CARTESIAN_POINT('Ctrl Pts',(-30.6998260242329,-43.690627791108,11.3977655520818));
#25302=CARTESIAN_POINT('Ctrl Pts',(-30.5027294109855,-43.7053049358871,
11.2969997378715));
#25303=CARTESIAN_POINT('',(-30.0406421838456,-43.7397150712088,11.5));
#25304=CARTESIAN_POINT('Ctrl Pts',(-30.5027294109855,-43.7053049358871,
11.2969997378715));
#25305=CARTESIAN_POINT('Ctrl Pts',(-30.242426966194,-43.7246888137001,11.4654707447276));
#25306=CARTESIAN_POINT('Ctrl Pts',(-30.0406421838456,-43.7397150712088,
11.5));
#25307=CARTESIAN_POINT('',(-30.0406421838456,-43.7397150712088,14.5));
#25308=CARTESIAN_POINT('Origin',(0.,0.,11.25));
#25309=CARTESIAN_POINT('',(-31.9903381491823,-42.8820272970037,11.5));
#25310=CARTESIAN_POINT('Origin',(0.,0.,11.5));
#25311=CARTESIAN_POINT('',(-32.140353293127,-42.5155015406339,11.2969997378715));
#25312=CARTESIAN_POINT('Ctrl Pts',(-32.140353293127,-42.5155015406339,11.2969997378715));
#25313=CARTESIAN_POINT('Ctrl Pts',(-32.0654882959165,-42.6984160718384,
11.3977655520825));
#25314=CARTESIAN_POINT('Ctrl Pts',(-31.9903381491823,-42.8820272970037,
11.5));
#25315=CARTESIAN_POINT('Ctrl Pts',(-32.140353293127,-42.515501540634,11.2969997378715));
#25316=CARTESIAN_POINT('Ctrl Pts',(-32.0253321418224,-42.4792652190273,
11.1987310576087));
#25317=CARTESIAN_POINT('Ctrl Pts',(-31.9132947806875,-42.4365064605718,
11.0971961933879));
#25318=CARTESIAN_POINT('Ctrl Pts',(-31.809565968283,-42.3928238374073,11.));
#25319=CARTESIAN_POINT('Ctrl Pts',(-30.5027294109855,-43.7053049358871,
11.2969997378715));
#25320=CARTESIAN_POINT('Ctrl Pts',(-30.5038101116606,-43.5847156812369,
11.1987310576087));
#25321=CARTESIAN_POINT('Ctrl Pts',(-30.4977655643985,-43.4649486358399,
11.0971961933879));
#25322=CARTESIAN_POINT('Ctrl Pts',(-30.4882748868283,-43.3527979999583,
11.));
#25323=CARTESIAN_POINT('Origin',(0.,0.,14.5));
#25324=CARTESIAN_POINT('',(-31.9903381491823,-42.8820272970037,24.2));
#25325=CARTESIAN_POINT('Origin',(0.,0.,24.2));
#25326=CARTESIAN_POINT('',(-31.9903381491823,-42.8820272970037,14.5));
#25327=CARTESIAN_POINT('Origin',(-32.1531051159017,-42.4843455428814,14.5));
#25328=CARTESIAN_POINT('',(-32.3158720826212,-42.0866637887591,24.2));
#25329=CARTESIAN_POINT('',(-32.2571123630091,-42.2302289656376,24.2));
#25330=CARTESIAN_POINT('',(-32.3158720826212,-42.0866637887591,11.5));
#25331=CARTESIAN_POINT('',(-32.3158720826212,-42.0866637887591,14.5));
#25332=CARTESIAN_POINT('Ctrl Pts',(-32.3158720826212,-42.0866637887591,
11.5));
#25333=CARTESIAN_POINT('Ctrl Pts',(-32.2392263355501,-42.2739291519686,
11.4654707447276));
#25334=CARTESIAN_POINT('Ctrl Pts',(-32.140353293127,-42.5155015406339,11.2969997378715));
#25335=CARTESIAN_POINT('Origin',(-33.443838774836,-41.4759138875076,14.5));
#25336=CARTESIAN_POINT('',(-33.8690845744085,-41.4141897191236,24.2));
#25337=CARTESIAN_POINT('',(-33.0185929752635,-41.5376380558916,24.2));
#25338=CARTESIAN_POINT('',(-33.1721089155843,-41.5153553108074,24.2));
#25339=CARTESIAN_POINT('',(-33.8690845744085,-41.4141897191236,11.5));
#25340=CARTESIAN_POINT('',(-33.8690845744085,-41.4141897191236,14.5));
#25341=CARTESIAN_POINT('',(-33.4771542514413,-41.4710781664027,11.2969997378715));
#25342=CARTESIAN_POINT('Ctrl Pts',(-33.8690845744085,-41.4141897191236,
11.5));
#25343=CARTESIAN_POINT('Ctrl Pts',(-33.6727469213825,-41.4426880096833,
11.3977655520828));
#25344=CARTESIAN_POINT('Ctrl Pts',(-33.4771542514413,-41.4710781664027,
11.2969997378715));
#25345=CARTESIAN_POINT('',(-33.0185929752635,-41.5376380558916,11.5));
#25346=CARTESIAN_POINT('Ctrl Pts',(-33.4771542514414,-41.4710781664027,
11.2969997378715));
#25347=CARTESIAN_POINT('Ctrl Pts',(-33.2188380412863,-41.5085726067192,
11.4654707447276));
#25348=CARTESIAN_POINT('Ctrl Pts',(-33.0185929752635,-41.5376380558916,
11.5));
#25349=CARTESIAN_POINT('',(-33.0185929752635,-41.5376380558916,14.5));
#25350=CARTESIAN_POINT('Origin',(0.,0.,11.25));
#25351=CARTESIAN_POINT('',(-34.9037103045182,-40.546035650582,11.5));
#25352=CARTESIAN_POINT('Origin',(0.,0.,11.5));
#25353=CARTESIAN_POINT('',(-35.1729694999764,-39.7299015085879,11.0622545443402));
#25354=CARTESIAN_POINT('Ctrl Pts',(-35.1729694999764,-39.7299015085879,
11.0622545443402));
#25355=CARTESIAN_POINT('Ctrl Pts',(-35.0388929451123,-40.1362922871065,
11.2776618075219));
#25356=CARTESIAN_POINT('Ctrl Pts',(-34.9037103045182,-40.546035650582,11.5));
#25357=CARTESIAN_POINT('Ctrl Pts',(-35.1966714489987,-39.6256775199017,
11.));
#25358=CARTESIAN_POINT('Ctrl Pts',(-35.1856729924399,-39.6612285891332,
11.0192759649605));
#25359=CARTESIAN_POINT('Ctrl Pts',(-35.1779404204734,-39.6963735392364,
11.0404458048696));
#25360=CARTESIAN_POINT('Ctrl Pts',(-35.1729694999764,-39.7299015085879,
11.0622545443403));
#25361=CARTESIAN_POINT('Ctrl Pts',(-33.4771542514414,-41.4710781664027,
11.2969997378715));
#25362=CARTESIAN_POINT('Ctrl Pts',(-33.4698204384081,-41.3507072752478,
11.1987310576087));
#25363=CARTESIAN_POINT('Ctrl Pts',(-33.4554360886017,-41.2316536226562,
11.0971961933879));
#25364=CARTESIAN_POINT('Ctrl Pts',(-33.4381452969578,-41.1204382162877,
11.));
#25365=CARTESIAN_POINT('Origin',(0.,0.,14.5));
#25366=CARTESIAN_POINT('',(-34.9037103045182,-40.546035650582,24.2));
#25367=CARTESIAN_POINT('Origin',(0.,0.,24.2));
#25368=CARTESIAN_POINT('',(-34.9037103045182,-40.546035650582,14.5));
#25369=CARTESIAN_POINT('Origin',(-36.2555847625695,-39.0419563844502,14.5));
#25370=CARTESIAN_POINT('',(-35.8356805007232,-39.1331938433149,11.0622545443404));
#25371=CARTESIAN_POINT('',(-35.8356805007232,-39.1331938433149,24.2));
#25372=CARTESIAN_POINT('',(-35.8356805007232,-39.1331938433149,14.5));
#25373=CARTESIAN_POINT('',(-36.6754890244158,-38.9507189255854,24.2));
#25374=CARTESIAN_POINT('',(-35.9872681182067,-39.1002566472175,24.2));
#25375=CARTESIAN_POINT('',(-36.6754890244158,-38.9507189255854,11.5));
#25376=CARTESIAN_POINT('',(-36.6754890244158,-38.9507189255854,14.5));
#25377=CARTESIAN_POINT('Ctrl Pts',(-36.6754890244158,-38.9507189255854,
11.5));
#25378=CARTESIAN_POINT('Ctrl Pts',(-36.3962351235305,-39.0113956526632,
11.3527407245755));
#25379=CARTESIAN_POINT('Ctrl Pts',(-36.1162869832672,-39.0722232251656,
11.206797012465));
#25380=CARTESIAN_POINT('Ctrl Pts',(-35.8356805007232,-39.1331938433149,
11.0622545443404));
#25381=CARTESIAN_POINT('Origin',(0.,0.,11.25));
#25382=CARTESIAN_POINT('Ctrl Pts',(-35.7295499336443,-39.1458715772075,
11.));
#25383=CARTESIAN_POINT('Ctrl Pts',(-35.7660555066417,-39.1386495482258,
11.0192757561174));
#25384=CARTESIAN_POINT('Ctrl Pts',(-35.8018169409009,-39.1346328909224,
11.0404460254343));
#25385=CARTESIAN_POINT('Ctrl Pts',(-35.8356805007232,-39.1331938433149,
11.0622545443404));
#25386=CARTESIAN_POINT('Origin',(0.,0.,11.5));
#25387=CARTESIAN_POINT('Origin',(0.,0.,11.25));
#25388=CARTESIAN_POINT('Origin',(0.,0.,11.5));
#25389=CARTESIAN_POINT('Origin',(0.,0.,11.25));
#25390=CARTESIAN_POINT('Origin',(0.,0.,11.5));
#25391=CARTESIAN_POINT('Origin',(0.,0.,14.5));
#25392=CARTESIAN_POINT('Origin',(0.,0.,24.2));
#25393=CARTESIAN_POINT('Origin',(0.,0.,14.5));
#25394=CARTESIAN_POINT('Origin',(0.,0.,24.2));
#25395=CARTESIAN_POINT('Origin',(0.,0.,14.5));
#25396=CARTESIAN_POINT('Origin',(0.,0.,24.2));
#25397=CARTESIAN_POINT('Origin',(-35.0383399022473,-40.137968579585,14.5));
#25398=CARTESIAN_POINT('',(-35.1729694999764,-39.729901508588,24.2));
#25399=CARTESIAN_POINT('',(-35.1243675165795,-39.8772158387497,24.2));
#25400=CARTESIAN_POINT('',(-35.1729694999764,-39.729901508588,14.5));
#25401=CARTESIAN_POINT('Origin',(-20.0789134070929,-49.6970546047798,11.25));
#25402=CARTESIAN_POINT('Origin',(-20.0789134070929,-49.6970546047798,11.5));
#25403=CARTESIAN_POINT('Origin',(-23.4966934678946,-48.1753608816353,11.25));
#25404=CARTESIAN_POINT('Origin',(-23.4966934678946,-48.1753608816353,11.5));
#25405=CARTESIAN_POINT('Origin',(-26.8,-46.4189616428459,11.25));
#25406=CARTESIAN_POINT('Origin',(-26.8,-46.4189616428459,11.5));
#25407=CARTESIAN_POINT('Origin',(-29.972739626032,-44.4364138889502,11.25));
#25408=CARTESIAN_POINT('Origin',(-29.972739626032,-44.4364138889502,11.5));
#25409=CARTESIAN_POINT('Origin',(-32.9994550774553,-42.2373763933203,11.25));
#25410=CARTESIAN_POINT('Origin',(-32.9994550774553,-42.2373763933203,11.5));
#25411=CARTESIAN_POINT('Origin',(-35.8654005008348,-39.8325626455883,11.));
#25412=CARTESIAN_POINT('Origin',(-35.8654005008348,-39.8325626455883,24.2));
#25413=CARTESIAN_POINT('Origin',(-32.9994550774553,-42.2373763933203,11.));
#25414=CARTESIAN_POINT('Origin',(-32.9994550774553,-42.2373763933203,24.2));
#25415=CARTESIAN_POINT('Origin',(-29.972739626032,-44.4364138889502,11.));
#25416=CARTESIAN_POINT('Origin',(-29.972739626032,-44.4364138889502,24.2));
#25417=CARTESIAN_POINT('Origin',(-26.8,-46.4189616428459,11.));
#25418=CARTESIAN_POINT('Origin',(-26.8,-46.4189616428459,24.2));
#25419=CARTESIAN_POINT('Origin',(-23.4966934678946,-48.1753608816353,11.));
#25420=CARTESIAN_POINT('Origin',(-23.4966934678946,-48.1753608816353,24.2));
#25421=CARTESIAN_POINT('Origin',(-20.0789134070929,-49.6970546047798,11.));
#25422=CARTESIAN_POINT('Origin',(-20.0789134070929,-49.6970546047798,24.2));
#25423=CARTESIAN_POINT('Origin',(-1.04073669728539,-53.2696785416253,14.5));
#25424=CARTESIAN_POINT('',(-1.012107219952,-53.287388939917,11.2969997378715));
#25425=CARTESIAN_POINT('',(-0.675303984907606,-53.495737816465,11.5));
#25426=CARTESIAN_POINT('Ctrl Pts',(-1.012107219952,-53.287388939917,11.2969997378715));
#25427=CARTESIAN_POINT('Ctrl Pts',(-0.844025701051962,-53.3913653629068,
11.397765552083));
#25428=CARTESIAN_POINT('Ctrl Pts',(-0.675303984907606,-53.495737816465,
11.5));
#25429=CARTESIAN_POINT('',(-0.675303984907606,-53.495737816465,24.2));
#25430=CARTESIAN_POINT('',(-0.675303984907606,-53.495737816465,14.5));
#25431=CARTESIAN_POINT('',(-1.40616940966318,-53.0436192667856,24.2));
#25432=CARTESIAN_POINT('',(-1.27424630420036,-53.1252278380639,24.2));
#25433=CARTESIAN_POINT('',(-1.40616940966318,-53.0436192667856,11.5));
#25434=CARTESIAN_POINT('',(-1.40616940966318,-53.0436192667856,14.5));
#25435=CARTESIAN_POINT('Ctrl Pts',(-1.40616940966318,-53.0436192667856,
11.5));
#25436=CARTESIAN_POINT('Ctrl Pts',(-1.23408987897642,-53.1500688883006,
11.4654707447276));
#25437=CARTESIAN_POINT('Ctrl Pts',(-1.012107219952,-53.287388939917,11.2969997378715));
#25438=CARTESIAN_POINT('Origin',(-1.87061302325404,-53.5673483282235,11.25));
#25439=CARTESIAN_POINT('',(-2.29739178302175,-53.0124970957196,11.5));
#25440=CARTESIAN_POINT('Origin',(-1.87061302325404,-53.5673483282235,11.5));
#25441=CARTESIAN_POINT('',(-2.70749856984771,-53.2281845693891,11.2969997378715));
#25442=CARTESIAN_POINT('Ctrl Pts',(-2.70749856984771,-53.2281845693891,
11.2969997378715));
#25443=CARTESIAN_POINT('Ctrl Pts',(-2.47647768684878,-53.1066837500425,
11.4654707447276));
#25444=CARTESIAN_POINT('Ctrl Pts',(-2.29739178302175,-53.0124970957196,
11.5));
#25445=CARTESIAN_POINT('Ctrl Pts',(-2.88204065427986,-52.9215820026866,
11.));
#25446=CARTESIAN_POINT('Ctrl Pts',(-2.83065842287485,-53.0217204288036,
11.0971961933879));
#25447=CARTESIAN_POINT('Ctrl Pts',(-2.77231762509644,-53.1264917656727,
11.1987310576087));
#25448=CARTESIAN_POINT('Ctrl Pts',(-2.70749856984771,-53.2281845693891,
11.2969997378715));
#25449=CARTESIAN_POINT('Ctrl Pts',(-1.01210721995201,-53.287388939917,11.2969997378715));
#25450=CARTESIAN_POINT('Ctrl Pts',(-0.940352329271679,-53.190465403485,
11.1987310576086));
#25451=CARTESIAN_POINT('Ctrl Pts',(-0.874845167735035,-53.0900189326552,
11.0971961933879));
#25452=CARTESIAN_POINT('Ctrl Pts',(-0.816602797371071,-52.9937086819872,
11.));
#25453=CARTESIAN_POINT('Origin',(-1.87061302325404,-53.5673483282235,11.));
#25454=CARTESIAN_POINT('',(-2.29739178302175,-53.0124970957196,24.2));
#25455=CARTESIAN_POINT('Origin',(-1.87061302325404,-53.5673483282235,24.2));
#25456=CARTESIAN_POINT('',(-2.29739178302175,-53.0124970957196,14.5));
#25457=CARTESIAN_POINT('Origin',(-2.67770341754862,-53.2125144041213,14.5));
#25458=CARTESIAN_POINT('',(-3.05801505207549,-53.412531712523,24.2));
#25459=CARTESIAN_POINT('',(-2.43468625658981,-53.0847043819776,24.2));
#25460=CARTESIAN_POINT('',(-3.05801505207549,-53.412531712523,11.5));
#25461=CARTESIAN_POINT('',(-3.05801505207549,-53.412531712523,14.5));
#25462=CARTESIAN_POINT('Ctrl Pts',(-3.05801505207549,-53.412531712523,11.5));
#25463=CARTESIAN_POINT('Ctrl Pts',(-2.88242367923521,-53.320182936978,11.3977655520828));
#25464=CARTESIAN_POINT('Ctrl Pts',(-2.70749856984771,-53.2281845693891,
11.2969997378715));
#25465=CARTESIAN_POINT('Origin',(0.,0.,11.25));
#25466=CARTESIAN_POINT('',(-4.40533300875789,-53.318318063138,11.5));
#25467=CARTESIAN_POINT('Origin',(0.,0.,11.5));
#25468=CARTESIAN_POINT('',(-4.72678212511286,-53.0869825079594,11.2969997378715));
#25469=CARTESIAN_POINT('Ctrl Pts',(-4.72678212511286,-53.0869825079594,
11.2969997378715));
#25470=CARTESIAN_POINT('Ctrl Pts',(-4.56636307296501,-53.2024304236689,
11.3977655520833));
#25471=CARTESIAN_POINT('Ctrl Pts',(-4.40533300875789,-53.318318063138,11.5));
#25472=CARTESIAN_POINT('Ctrl Pts',(-4.72678212511287,-53.0869825079594,
11.2969997378715));
#25473=CARTESIAN_POINT('Ctrl Pts',(-4.64844098161556,-52.9953004405385,
11.1987310576086));
#25474=CARTESIAN_POINT('Ctrl Pts',(-4.57608660062692,-52.8996682008571,
11.0971961933879));
#25475=CARTESIAN_POINT('Ctrl Pts',(-4.51126784227787,-52.8076553394982,
11.));
#25476=CARTESIAN_POINT('Origin',(-4.75410644754494,-53.0673181599239,14.5));
#25477=CARTESIAN_POINT('',(-4.40533300875789,-53.318318063138,24.2));
#25478=CARTESIAN_POINT('',(-4.40533300875789,-53.318318063138,14.5));
#25479=CARTESIAN_POINT('',(-5.10287988633199,-52.8163182567097,24.2));
#25480=CARTESIAN_POINT('',(-4.97697086508331,-52.9069305242525,24.2));
#25481=CARTESIAN_POINT('',(-5.10287988633199,-52.8163182567097,11.5));
#25482=CARTESIAN_POINT('',(-5.10287988633199,-52.8163182567097,14.5));
#25483=CARTESIAN_POINT('Ctrl Pts',(-5.10287988633199,-52.8163182567097,
11.5));
#25484=CARTESIAN_POINT('Ctrl Pts',(-4.93864508296158,-52.9345122335611,
11.4654707447276));
#25485=CARTESIAN_POINT('Ctrl Pts',(-4.72678212511286,-53.0869825079594,
11.2969997378715));
#25486=CARTESIAN_POINT('Origin',(-5.60272563114622,-53.3063735917395,11.25));
#25487=CARTESIAN_POINT('',(-5.98976031387286,-52.7231033676009,11.5));
#25488=CARTESIAN_POINT('Origin',(-5.60272563114622,-53.3063735917395,11.5));
#25489=CARTESIAN_POINT('',(-6.413913698772,-52.9096578341174,11.2969997378716));
#25490=CARTESIAN_POINT('Ctrl Pts',(-6.413913698772,-52.9096578341174,11.2969997378716));
#25491=CARTESIAN_POINT('Ctrl Pts',(-6.17498010231831,-52.8045681868194,
11.4654707447277));
#25492=CARTESIAN_POINT('Ctrl Pts',(-5.98976031387286,-52.7231033676009,
11.5));
#25493=CARTESIAN_POINT('Ctrl Pts',(-6.41391369877199,-52.9096578341175,
11.2969997378716));
#25494=CARTESIAN_POINT('Ctrl Pts',(-6.47148112666751,-52.8036912002343,
11.1987310576087));
#25495=CARTESIAN_POINT('Ctrl Pts',(-6.52237133018529,-52.6951054327476,
11.0971961933879));
#25496=CARTESIAN_POINT('Ctrl Pts',(-6.56664309356486,-52.5916266955277,
11.));
#25497=CARTESIAN_POINT('Origin',(-5.60272563114622,-53.3063735917395,11.));
#25498=CARTESIAN_POINT('',(-5.98976031387285,-52.7231033676009,24.2));
#25499=CARTESIAN_POINT('Origin',(-5.60272563114622,-53.3063735917395,24.2));
#25500=CARTESIAN_POINT('',(-5.98976031387285,-52.7231033676009,14.5));
#25501=CARTESIAN_POINT('Origin',(-6.38309803049425,-52.8961042453437,14.5));
#25502=CARTESIAN_POINT('',(-6.77643574711566,-53.0691051230866,24.2));
#25503=CARTESIAN_POINT('',(-6.13175727067173,-52.785557582198,24.2));
#25504=CARTESIAN_POINT('',(-6.77643574711566,-53.0691051230866,11.5));
#25505=CARTESIAN_POINT('',(-6.77643574711566,-53.0691051230866,14.5));
#25506=CARTESIAN_POINT('Ctrl Pts',(-6.77643574711566,-53.0691051230866,
11.5));
#25507=CARTESIAN_POINT('Ctrl Pts',(-6.594830181098,-52.9892299395067,11.3977655520829));
#25508=CARTESIAN_POINT('Ctrl Pts',(-6.413913698772,-52.9096578341174,11.2969997378716));
#25509=CARTESIAN_POINT('Origin',(-8.44431466907315,-52.6064191384554,14.5));
#25510=CARTESIAN_POINT('',(-8.41842862289463,-52.6279416335078,11.2969997378715));
#25511=CARTESIAN_POINT('',(-8.11389969301203,-52.8811368237459,11.5));
#25512=CARTESIAN_POINT('Ctrl Pts',(-8.41842862289463,-52.6279416335078,
11.2969997378715));
#25513=CARTESIAN_POINT('Ctrl Pts',(-8.26645358299721,-52.7542985912954,
11.3977655520826));
#25514=CARTESIAN_POINT('Ctrl Pts',(-8.11389969301203,-52.8811368237459,
11.5));
#25515=CARTESIAN_POINT('',(-8.11389969301203,-52.8811368237459,24.2));
#25516=CARTESIAN_POINT('',(-8.11389969301203,-52.8811368237459,14.5));
#25517=CARTESIAN_POINT('',(-8.77472964513427,-52.3317014531649,24.2));
#25518=CARTESIAN_POINT('',(-8.65544812419494,-52.430875963113,24.2));
#25519=CARTESIAN_POINT('',(-8.77472964513427,-52.3317014531649,11.5));
#25520=CARTESIAN_POINT('',(-8.77472964513427,-52.3317014531649,14.5));
#25521=CARTESIAN_POINT('Ctrl Pts',(-8.77472964513427,-52.3317014531649,
11.5));
#25522=CARTESIAN_POINT('Ctrl Pts',(-8.6191397045334,-52.4610639561783,11.4654707447276));
#25523=CARTESIAN_POINT('Ctrl Pts',(-8.41842862289463,-52.6279416335078,
11.2969997378715));
#25524=CARTESIAN_POINT('Origin',(-9.30754232294747,-52.7856955614544,11.25));
#25525=CARTESIAN_POINT('',(-9.65294733456354,-52.1768479795831,11.5));
#25526=CARTESIAN_POINT('Origin',(-9.30754232294747,-52.7856955614544,11.5));
#25527=CARTESIAN_POINT('',(-10.0890808848803,-52.3333605643381,11.2969997378715));
#25528=CARTESIAN_POINT('Ctrl Pts',(-10.0890808848803,-52.3333605643381,
11.2969997378715));
#25529=CARTESIAN_POINT('Ctrl Pts',(-9.84339863543634,-52.2451940752868,
11.4654707447276));
#25530=CARTESIAN_POINT('Ctrl Pts',(-9.65294733456354,-52.1768479795831,
11.5));
#25531=CARTESIAN_POINT('Ctrl Pts',(-10.0890808848803,-52.3333605643381,
11.2969997378715));
#25532=CARTESIAN_POINT('Ctrl Pts',(-10.1391162227005,-52.2236363590767,
11.1987310576086));
#25533=CARTESIAN_POINT('Ctrl Pts',(-10.1823079000016,-52.1117651799167,
11.0971961933879));
#25534=CARTESIAN_POINT('Ctrl Pts',(-10.2192535077747,-52.0054502696,11.));
#25535=CARTESIAN_POINT('Ctrl Pts',(-8.41842862289464,-52.6279416335078,
11.2969997378715));
#25536=CARTESIAN_POINT('Ctrl Pts',(-8.33388289675662,-52.5419477009147,
11.1987310576086));
#25537=CARTESIAN_POINT('Ctrl Pts',(-8.25503379958712,-52.4515956030403,
11.0971961933879));
#25538=CARTESIAN_POINT('Ctrl Pts',(-8.18395444372813,-52.3643284084021,
11.));
#25539=CARTESIAN_POINT('Origin',(-9.30754232294747,-52.7856955614544,11.));
#25540=CARTESIAN_POINT('',(-9.65294733456354,-52.1768479795831,24.2));
#25541=CARTESIAN_POINT('Origin',(-9.30754232294747,-52.7856955614544,24.2));
#25542=CARTESIAN_POINT('',(-9.65294733456355,-52.1768479795831,14.5));
#25543=CARTESIAN_POINT('Origin',(-10.0573948314625,-52.3219895837806,14.5));
#25544=CARTESIAN_POINT('',(-10.4618423283614,-52.4671311879781,24.2));
#25545=CARTESIAN_POINT('',(-9.79895497969307,-52.2292448518636,24.2));
#25546=CARTESIAN_POINT('',(-10.4618423283614,-52.4671311879781,11.5));
#25547=CARTESIAN_POINT('',(-10.4618423283614,-52.4671311879781,14.5));
#25548=CARTESIAN_POINT('Ctrl Pts',(-10.4618423283614,-52.4671311879781,
11.5));
#25549=CARTESIAN_POINT('Ctrl Pts',(-10.275107333229,-52.4001187402287,11.397765552083));
#25550=CARTESIAN_POINT('Ctrl Pts',(-10.0890808848803,-52.3333605643381,
11.2969997378715));
#25551=CARTESIAN_POINT('Origin',(-12.0933830383532,-51.8892269309232,14.5));
#25552=CARTESIAN_POINT('',(-12.0690613826431,-51.9125027175599,11.2969997378715));
#25553=CARTESIAN_POINT('',(-11.7829362735682,-52.1863240013419,11.5));
#25554=CARTESIAN_POINT('Ctrl Pts',(-12.0690613826431,-51.9125027175599,
11.2969997378715));
#25555=CARTESIAN_POINT('Ctrl Pts',(-11.9262707621126,-52.0491531190297,
11.3977655520828));
#25556=CARTESIAN_POINT('Ctrl Pts',(-11.7829362735682,-52.1863240013419,
11.5));
#25557=CARTESIAN_POINT('',(-11.7829362735682,-52.1863240013419,24.2));
#25558=CARTESIAN_POINT('',(-11.7829362735682,-52.1863240013419,14.5));
#25559=CARTESIAN_POINT('',(-12.4038298031382,-51.5921298605045,24.2));
#25560=CARTESIAN_POINT('',(-12.2917569100881,-51.6993834446145,24.2));
#25561=CARTESIAN_POINT('',(-12.4038298031382,-51.5921298605045,11.5));
#25562=CARTESIAN_POINT('',(-12.4038298031382,-51.5921298605045,14.5));
#25563=CARTESIAN_POINT('Ctrl Pts',(-12.4038298031382,-51.5921298605045,
11.5));
#25564=CARTESIAN_POINT('Ctrl Pts',(-12.2576427438576,-51.7320306485686,
11.4654707447276));
#25565=CARTESIAN_POINT('Ctrl Pts',(-12.0690613826431,-51.9125027175599,
11.2969997378715));
#25566=CARTESIAN_POINT('Origin',(-12.9670136041422,-52.0078509283934,11.25));
#25567=CARTESIAN_POINT('',(-13.269106166151,-51.3763922330071,11.5));
#25568=CARTESIAN_POINT('Origin',(-12.9670136041422,-52.0078509283934,11.5));
#25569=CARTESIAN_POINT('',(-13.7150950830682,-51.5021004224203,11.2969997378715));
#25570=CARTESIAN_POINT('Ctrl Pts',(-13.7150950830682,-51.5021004224203,
11.2969997378715));
#25571=CARTESIAN_POINT('Ctrl Pts',(-13.4638611198574,-51.4312866298879,
11.4654707447276));
#25572=CARTESIAN_POINT('Ctrl Pts',(-13.269106166151,-51.3763922330071,11.5));
#25573=CARTESIAN_POINT('Ctrl Pts',(-13.7150950830682,-51.5021004224203,
11.2969997378715));
#25574=CARTESIAN_POINT('Ctrl Pts',(-13.7573545636769,-51.3891532110793,
11.1987310576086));
#25575=CARTESIAN_POINT('Ctrl Pts',(-13.7926372892511,-51.2745416453855,
11.0971961933879));
#25576=CARTESIAN_POINT('Ctrl Pts',(-13.8220767461304,-51.1659085175284,
11.));
#25577=CARTESIAN_POINT('Ctrl Pts',(-12.0690613826432,-51.9125027175599,
11.2969997378715));
#25578=CARTESIAN_POINT('Ctrl Pts',(-11.9787229721437,-51.8326158735901,
11.1987310576086));
#25579=CARTESIAN_POINT('Ctrl Pts',(-11.8937633036688,-51.7479841038615,
11.0971961933879));
#25580=CARTESIAN_POINT('Ctrl Pts',(-11.8167696417768,-51.6658877329441,
11.));
#25581=CARTESIAN_POINT('Origin',(-12.9670136041422,-52.0078509283934,11.));
#25582=CARTESIAN_POINT('',(-13.269106166151,-51.3763922330071,24.2));
#25583=CARTESIAN_POINT('Origin',(-12.9670136041422,-52.0078509283934,24.2));
#25584=CARTESIAN_POINT('',(-13.269106166151,-51.3763922330071,14.5));
#25585=CARTESIAN_POINT('Origin',(-15.6835336610931,-50.9192356256703,14.5));
#25586=CARTESIAN_POINT('',(-15.97249974917,-50.6012065971863,11.0622545443402));
#25587=CARTESIAN_POINT('',(-15.3945675730164,-51.2372646541541,11.5));
#25588=CARTESIAN_POINT('Ctrl Pts',(-15.97249974917,-50.6012065971863,11.0622545443402));
#25589=CARTESIAN_POINT('Ctrl Pts',(-15.6847207004672,-50.9179291990878,
11.2776618075209));
#25590=CARTESIAN_POINT('Ctrl Pts',(-15.3945675730164,-51.2372646541541,
11.5));
#25591=CARTESIAN_POINT('',(-15.3945675730164,-51.2372646541541,24.2));
#25592=CARTESIAN_POINT('',(-15.3945675730164,-51.2372646541541,14.5));
#25593=CARTESIAN_POINT('',(-15.9724997491699,-50.6012065971864,24.2));
#25594=CARTESIAN_POINT('',(-15.8681814918784,-50.7160167267776,24.2));
#25595=CARTESIAN_POINT('',(-15.9724997491699,-50.6012065971864,14.5));
#25596=CARTESIAN_POINT('Origin',(0.,0.,14.5));
#25597=CARTESIAN_POINT('',(-14.0962798654037,-51.6095426636995,11.5));
#25598=CARTESIAN_POINT('Origin',(0.,0.,11.5));
#25599=CARTESIAN_POINT('',(-14.0962798654037,-51.6095426636995,24.2));
#25600=CARTESIAN_POINT('',(-14.0962798654037,-51.6095426636995,14.5));
#25601=CARTESIAN_POINT('Origin',(0.,0.,24.2));
#25602=CARTESIAN_POINT('Origin',(0.,0.,11.25));
#25603=CARTESIAN_POINT('Ctrl Pts',(-16.0365442723228,-50.5156336969243,
11.));
#25604=CARTESIAN_POINT('Ctrl Pts',(-16.0120367597354,-50.5436377394353,
11.0192759649605));
#25605=CARTESIAN_POINT('Ctrl Pts',(-15.9906779647135,-50.5725991285972,
11.0404458048696));
#25606=CARTESIAN_POINT('Ctrl Pts',(-15.97249974917,-50.6012065971862,11.0622545443403));
#25607=CARTESIAN_POINT('Ctrl Pts',(-14.0962798654037,-51.6095426636995,
11.5));
#25608=CARTESIAN_POINT('Ctrl Pts',(-13.9053251952808,-51.5557194296894,
11.3977655520823));
#25609=CARTESIAN_POINT('Ctrl Pts',(-13.7150950830682,-51.5021004224203,
11.2969997378715));
#25610=CARTESIAN_POINT('Origin',(-13.6826930157773,-51.4929674483533,14.5));
#25611=CARTESIAN_POINT('',(-13.4184131650408,-51.4184764906763,24.2));
#25612=CARTESIAN_POINT('Origin',(19.1972756843392,-49.7011709228329,14.5));
#25613=CARTESIAN_POINT('',(18.9311980867048,-50.0385825039234,24.2));
#25614=CARTESIAN_POINT('',(19.4633532819736,-49.3637593417425,24.2));
#25615=CARTESIAN_POINT('',(19.3672978885042,-49.485566673404,24.2));
#25616=CARTESIAN_POINT('',(18.9311980867048,-50.0385825039234,11.5));
#25617=CARTESIAN_POINT('',(18.9311980867048,-50.0385825039234,14.5));
#25618=CARTESIAN_POINT('',(19.4633532819737,-49.3637593417424,11.0622545443403));
#25619=CARTESIAN_POINT('Ctrl Pts',(18.9311980867048,-50.0385825039234,11.5));
#25620=CARTESIAN_POINT('Ctrl Pts',(19.1983687004362,-49.6997848749554,11.2776618075187));
#25621=CARTESIAN_POINT('Ctrl Pts',(19.4633532819737,-49.3637593417424,11.0622545443403));
#25622=CARTESIAN_POINT('',(19.4633532819736,-49.3637593417425,14.5));
#25623=CARTESIAN_POINT('Origin',(0.,0.,11.25));
#25624=CARTESIAN_POINT('',(17.6620417438945,-50.5005176353365,11.5));
#25625=CARTESIAN_POINT('Origin',(0.,0.,11.5));
#25626=CARTESIAN_POINT('',(17.274290716648,-50.4199272242177,11.2969997378715));
#25627=CARTESIAN_POINT('Ctrl Pts',(17.274290716648,-50.4199272242177,11.2969997378715));
#25628=CARTESIAN_POINT('Ctrl Pts',(17.4677977107421,-50.4601458364523,11.397765552083));
#25629=CARTESIAN_POINT('Ctrl Pts',(17.6620417438945,-50.5005176353365,11.5));
#25630=CARTESIAN_POINT('Ctrl Pts',(17.274290716648,-50.4199272242177,11.2969997378715));
#25631=CARTESIAN_POINT('Ctrl Pts',(17.3085684561035,-50.3043072742572,11.1987310576087));
#25632=CARTESIAN_POINT('Ctrl Pts',(17.3357703360584,-50.1875136980569,11.0971961933879));
#25633=CARTESIAN_POINT('Ctrl Pts',(17.3575602159693,-50.0770916023385,11.));
#25634=CARTESIAN_POINT('Ctrl Pts',(19.4633532819737,-49.3637593417423,11.0622545443403));
#25635=CARTESIAN_POINT('Ctrl Pts',(19.4794916601662,-49.3339535112937,11.0404458048696));
#25636=CARTESIAN_POINT('Ctrl Pts',(19.4987781818543,-49.3035727563959,11.0192759649605));
#25637=CARTESIAN_POINT('Ctrl Pts',(19.5212725321166,-49.2739273726667,11.));
#25638=CARTESIAN_POINT('Origin',(0.,0.,14.5));
#25639=CARTESIAN_POINT('',(17.6620417438945,-50.5005176353365,24.2));
#25640=CARTESIAN_POINT('Origin',(0.,0.,24.2));
#25641=CARTESIAN_POINT('',(17.6620417438945,-50.5005176353365,14.5));
#25642=CARTESIAN_POINT('Origin',(17.2413304950986,-50.4130767515726,14.5));
#25643=CARTESIAN_POINT('',(16.8206192463027,-50.3256358678088,24.2));
#25644=CARTESIAN_POINT('',(16.9724981902626,-50.3572024805937,24.2));
#25645=CARTESIAN_POINT('',(16.8206192463027,-50.3256358678088,11.5));
#25646=CARTESIAN_POINT('',(16.8206192463027,-50.3256358678088,14.5));
#25647=CARTESIAN_POINT('Ctrl Pts',(16.8206192463027,-50.3256358678088,11.5));
#25648=CARTESIAN_POINT('Ctrl Pts',(17.0187290262849,-50.366811125883,11.4654707447276));
#25649=CARTESIAN_POINT('Ctrl Pts',(17.274290716648,-50.4199272242177,11.2969997378715));
#25650=CARTESIAN_POINT('Origin',(15.6835336610932,-50.9192356256702,14.5));
#25651=CARTESIAN_POINT('',(15.3945675730165,-51.2372646541541,24.2));
#25652=CARTESIAN_POINT('',(15.9724997491699,-50.6012065971864,24.2));
#25653=CARTESIAN_POINT('',(15.8681814918784,-50.7160167267776,24.2));
#25654=CARTESIAN_POINT('',(15.3945675730165,-51.2372646541541,11.5));
#25655=CARTESIAN_POINT('',(15.3945675730165,-51.2372646541541,14.5));
#25656=CARTESIAN_POINT('',(15.6608948885133,-50.9441513065986,11.2969997378716));
#25657=CARTESIAN_POINT('Ctrl Pts',(15.3945675730165,-51.2372646541541,11.5));
#25658=CARTESIAN_POINT('Ctrl Pts',(15.527984348901,-51.0904294047295,11.3977655520823));
#25659=CARTESIAN_POINT('Ctrl Pts',(15.6608948885133,-50.9441513065986,11.2969997378716));
#25660=CARTESIAN_POINT('',(15.9724997491699,-50.6012065971864,11.5));
#25661=CARTESIAN_POINT('Ctrl Pts',(15.6608948885133,-50.9441513065986,11.2969997378716));
#25662=CARTESIAN_POINT('Ctrl Pts',(15.8364277798678,-50.7509640877247,11.4654707447277));
#25663=CARTESIAN_POINT('Ctrl Pts',(15.9724997491699,-50.6012065971864,11.5));
#25664=CARTESIAN_POINT('',(15.9724997491699,-50.6012065971864,14.5));
#25665=CARTESIAN_POINT('Origin',(0.,0.,11.25));
#25666=CARTESIAN_POINT('',(14.0962798654032,-51.6095426636996,11.5));
#25667=CARTESIAN_POINT('Origin',(0.,0.,11.5));
#25668=CARTESIAN_POINT('',(13.7150950830682,-51.5021004224204,11.2969997378716));
#25669=CARTESIAN_POINT('Ctrl Pts',(13.7150950830682,-51.5021004224204,11.2969997378716));
#25670=CARTESIAN_POINT('Ctrl Pts',(13.9053251952827,-51.5557194296901,11.3977655520835));
#25671=CARTESIAN_POINT('Ctrl Pts',(14.0962798654032,-51.6095426636996,11.5));
#25672=CARTESIAN_POINT('Ctrl Pts',(13.7150950830682,-51.5021004224204,11.2969997378716));
#25673=CARTESIAN_POINT('Ctrl Pts',(13.7573545636769,-51.3891532110794,11.1987310576087));
#25674=CARTESIAN_POINT('Ctrl Pts',(13.792637289251,-51.2745416453855,11.0971961933879));
#25675=CARTESIAN_POINT('Ctrl Pts',(13.8220767461304,-51.1659085175284,11.));
#25676=CARTESIAN_POINT('Ctrl Pts',(15.6608948885133,-50.9441513065987,11.2969997378716));
#25677=CARTESIAN_POINT('Ctrl Pts',(15.5652039133075,-50.8707607519257,11.1987310576087));
#25678=CARTESIAN_POINT('Ctrl Pts',(15.474547588492,-50.7922616278179,11.0971961933879));
#25679=CARTESIAN_POINT('Ctrl Pts',(15.3920147259482,-50.7157360458881,11.));
#25680=CARTESIAN_POINT('Origin',(0.,0.,14.5));
#25681=CARTESIAN_POINT('',(14.0962798654032,-51.6095426636996,24.2));
#25682=CARTESIAN_POINT('Origin',(0.,0.,24.2));
#25683=CARTESIAN_POINT('',(14.0962798654032,-51.6095426636996,14.5));
#25684=CARTESIAN_POINT('Origin',(13.682693015777,-51.4929674483533,14.5));
#25685=CARTESIAN_POINT('',(13.2691061661508,-51.3763922330071,24.2));
#25686=CARTESIAN_POINT('',(13.4184131650408,-51.4184764906764,24.2));
#25687=CARTESIAN_POINT('',(13.2691061661508,-51.3763922330071,11.5));
#25688=CARTESIAN_POINT('',(13.2691061661508,-51.3763922330071,14.5));
#25689=CARTESIAN_POINT('Ctrl Pts',(13.2691061661508,-51.3763922330071,11.5));
#25690=CARTESIAN_POINT('Ctrl Pts',(13.4638611198572,-51.4312866298879,11.4654707447276));
#25691=CARTESIAN_POINT('Ctrl Pts',(13.7150950830682,-51.5021004224204,11.2969997378716));
#25692=CARTESIAN_POINT('Origin',(12.0933830383532,-51.8892269309232,14.5));
#25693=CARTESIAN_POINT('',(11.7829362735681,-52.1863240013419,24.2));
#25694=CARTESIAN_POINT('',(12.4038298031382,-51.5921298605045,24.2));
#25695=CARTESIAN_POINT('',(12.2917569100881,-51.6993834446145,24.2));
#25696=CARTESIAN_POINT('',(11.7829362735681,-52.1863240013419,11.5));
#25697=CARTESIAN_POINT('',(11.7829362735681,-52.1863240013419,14.5));
#25698=CARTESIAN_POINT('',(12.0690613826431,-51.9125027175599,11.2969997378715));
#25699=CARTESIAN_POINT('Ctrl Pts',(11.7829362735681,-52.1863240013419,11.5));
#25700=CARTESIAN_POINT('Ctrl Pts',(11.9262707621134,-52.049153119029,11.3977655520823));
#25701=CARTESIAN_POINT('Ctrl Pts',(12.0690613826431,-51.9125027175599,11.2969997378715));
#25702=CARTESIAN_POINT('',(12.4038298031382,-51.5921298605045,11.5));
#25703=CARTESIAN_POINT('Ctrl Pts',(12.0690613826431,-51.9125027175599,11.2969997378715));
#25704=CARTESIAN_POINT('Ctrl Pts',(12.2576427438576,-51.7320306485686,11.4654707447276));
#25705=CARTESIAN_POINT('Ctrl Pts',(12.4038298031382,-51.5921298605045,11.5));
#25706=CARTESIAN_POINT('',(12.4038298031382,-51.5921298605045,14.5));
#25707=CARTESIAN_POINT('Origin',(0.,0.,11.25));
#25708=CARTESIAN_POINT('',(10.4618423283611,-52.4671311879782,11.5));
#25709=CARTESIAN_POINT('Origin',(0.,0.,11.5));
#25710=CARTESIAN_POINT('',(10.0890808848802,-52.3333605643381,11.2969997378715));
#25711=CARTESIAN_POINT('Ctrl Pts',(10.0890808848802,-52.3333605643381,11.2969997378715));
#25712=CARTESIAN_POINT('Ctrl Pts',(10.2751073332268,-52.400118740228,11.3977655520819));
#25713=CARTESIAN_POINT('Ctrl Pts',(10.4618423283611,-52.4671311879782,11.5));
#25714=CARTESIAN_POINT('Ctrl Pts',(10.0890808848802,-52.3333605643381,11.2969997378715));
#25715=CARTESIAN_POINT('Ctrl Pts',(10.1391162227005,-52.2236363590767,11.1987310576087));
#25716=CARTESIAN_POINT('Ctrl Pts',(10.1823079000016,-52.1117651799167,11.0971961933879));
#25717=CARTESIAN_POINT('Ctrl Pts',(10.2192535077747,-52.0054502696,11.));
#25718=CARTESIAN_POINT('Ctrl Pts',(12.0690613826431,-51.9125027175599,11.2969997378715));
#25719=CARTESIAN_POINT('Ctrl Pts',(11.9787229721437,-51.8326158735901,11.1987310576086));
#25720=CARTESIAN_POINT('Ctrl Pts',(11.8937633036688,-51.7479841038615,11.0971961933879));
#25721=CARTESIAN_POINT('Ctrl Pts',(11.8167696417768,-51.6658877329441,11.));
#25722=CARTESIAN_POINT('Origin',(0.,0.,14.5));
#25723=CARTESIAN_POINT('',(10.4618423283611,-52.4671311879782,24.2));
#25724=CARTESIAN_POINT('Origin',(0.,0.,24.2));
#25725=CARTESIAN_POINT('',(10.4618423283611,-52.4671311879782,14.5));
#25726=CARTESIAN_POINT('Origin',(10.0573948314623,-52.3219895837806,14.5));
#25727=CARTESIAN_POINT('',(9.65294733456344,-52.176847979583,24.2));
#25728=CARTESIAN_POINT('',(9.79895497969302,-52.2292448518636,24.2));
#25729=CARTESIAN_POINT('',(9.65294733456344,-52.176847979583,11.5));
#25730=CARTESIAN_POINT('',(9.65294733456345,-52.176847979583,14.5));
#25731=CARTESIAN_POINT('Ctrl Pts',(9.65294733456344,-52.176847979583,11.5));
#25732=CARTESIAN_POINT('Ctrl Pts',(9.84339863543623,-52.2451940752868,11.4654707447276));
#25733=CARTESIAN_POINT('Ctrl Pts',(10.0890808848802,-52.3333605643381,11.2969997378715));
#25734=CARTESIAN_POINT('Origin',(8.44431466907313,-52.6064191384554,14.5));
#25735=CARTESIAN_POINT('',(8.11389969301201,-52.8811368237459,24.2));
#25736=CARTESIAN_POINT('',(8.77472964513425,-52.3317014531649,24.2));
#25737=CARTESIAN_POINT('',(8.65544812419492,-52.430875963113,24.2));
#25738=CARTESIAN_POINT('',(8.11389969301201,-52.8811368237459,11.5));
#25739=CARTESIAN_POINT('',(8.11389969301201,-52.8811368237459,14.5));
#25740=CARTESIAN_POINT('',(8.41842862289461,-52.6279416335077,11.2969997378715));
#25741=CARTESIAN_POINT('Ctrl Pts',(8.11389969301201,-52.8811368237459,11.5));
#25742=CARTESIAN_POINT('Ctrl Pts',(8.2664535829971,-52.7542985912954,11.3977655520826));
#25743=CARTESIAN_POINT('Ctrl Pts',(8.41842862289461,-52.6279416335077,11.2969997378715));
#25744=CARTESIAN_POINT('',(8.77472964513425,-52.3317014531649,11.5));
#25745=CARTESIAN_POINT('Ctrl Pts',(8.41842862289461,-52.6279416335077,11.2969997378715));
#25746=CARTESIAN_POINT('Ctrl Pts',(8.61913970453333,-52.4610639561783,11.4654707447276));
#25747=CARTESIAN_POINT('Ctrl Pts',(8.77472964513425,-52.3317014531649,11.5));
#25748=CARTESIAN_POINT('',(8.77472964513425,-52.3317014531649,14.5));
#25749=CARTESIAN_POINT('Origin',(0.,0.,11.25));
#25750=CARTESIAN_POINT('',(6.77643574711564,-53.0691051230866,11.5));
#25751=CARTESIAN_POINT('Origin',(0.,0.,11.5));
#25752=CARTESIAN_POINT('',(6.41391369877197,-52.9096578341174,11.2969997378716));
#25753=CARTESIAN_POINT('Ctrl Pts',(6.41391369877197,-52.9096578341174,11.2969997378716));
#25754=CARTESIAN_POINT('Ctrl Pts',(6.59483018109746,-52.9892299395064,11.3977655520826));
#25755=CARTESIAN_POINT('Ctrl Pts',(6.77643574711564,-53.0691051230866,11.5));
#25756=CARTESIAN_POINT('Ctrl Pts',(6.41391369877197,-52.9096578341174,11.2969997378715));
#25757=CARTESIAN_POINT('Ctrl Pts',(6.47148112666749,-52.8036912002343,11.1987310576087));
#25758=CARTESIAN_POINT('Ctrl Pts',(6.52237133018527,-52.6951054327476,11.0971961933879));
#25759=CARTESIAN_POINT('Ctrl Pts',(6.56664309356484,-52.5916266955277,11.));
#25760=CARTESIAN_POINT('Ctrl Pts',(8.41842862289462,-52.6279416335077,11.2969997378715));
#25761=CARTESIAN_POINT('Ctrl Pts',(8.3338828967566,-52.5419477009146,11.1987310576086));
#25762=CARTESIAN_POINT('Ctrl Pts',(8.2550337995871,-52.4515956030403,11.0971961933879));
#25763=CARTESIAN_POINT('Ctrl Pts',(8.18395444372811,-52.3643284084021,11.));
#25764=CARTESIAN_POINT('Origin',(0.,0.,14.5));
#25765=CARTESIAN_POINT('',(6.77643574711564,-53.0691051230866,24.2));
#25766=CARTESIAN_POINT('Origin',(0.,0.,24.2));
#25767=CARTESIAN_POINT('',(6.77643574711564,-53.0691051230866,14.5));
#25768=CARTESIAN_POINT('Origin',(6.38309803049424,-52.8961042453437,14.5));
#25769=CARTESIAN_POINT('',(5.98976031387283,-52.7231033676009,24.2));
#25770=CARTESIAN_POINT('',(6.13175727067171,-52.785557582198,24.2));
#25771=CARTESIAN_POINT('',(5.98976031387283,-52.7231033676009,11.5));
#25772=CARTESIAN_POINT('',(5.98976031387283,-52.7231033676009,14.5));
#25773=CARTESIAN_POINT('Ctrl Pts',(5.98976031387283,-52.7231033676009,11.5));
#25774=CARTESIAN_POINT('Ctrl Pts',(6.17498010231827,-52.8045681868194,11.4654707447276));
#25775=CARTESIAN_POINT('Ctrl Pts',(6.41391369877197,-52.9096578341174,11.2969997378716));
#25776=CARTESIAN_POINT('Origin',(4.7541064475452,-53.0673181599238,14.5));
#25777=CARTESIAN_POINT('',(4.40533300875834,-53.318318063138,24.2));
#25778=CARTESIAN_POINT('',(5.10287988633206,-52.8163182567096,24.2));
#25779=CARTESIAN_POINT('',(4.97697086508333,-52.9069305242526,24.2));
#25780=CARTESIAN_POINT('',(4.40533300875834,-53.318318063138,11.5));
#25781=CARTESIAN_POINT('',(4.40533300875834,-53.318318063138,14.5));
#25782=CARTESIAN_POINT('',(4.72678212511292,-53.0869825079595,11.2969997378716));
#25783=CARTESIAN_POINT('Ctrl Pts',(4.40533300875834,-53.318318063138,11.5));
#25784=CARTESIAN_POINT('Ctrl Pts',(4.5663630729665,-53.202430423668,11.3977655520825));
#25785=CARTESIAN_POINT('Ctrl Pts',(4.72678212511292,-53.0869825079595,11.2969997378716));
#25786=CARTESIAN_POINT('',(5.10287988633206,-52.8163182567096,11.5));
#25787=CARTESIAN_POINT('Ctrl Pts',(4.72678212511292,-53.0869825079595,11.2969997378716));
#25788=CARTESIAN_POINT('Ctrl Pts',(4.93864508296159,-52.9345122335611,11.4654707447277));
#25789=CARTESIAN_POINT('Ctrl Pts',(5.10287988633206,-52.8163182567096,11.5));
#25790=CARTESIAN_POINT('',(5.10287988633206,-52.8163182567096,14.5));
#25791=CARTESIAN_POINT('Origin',(0.,0.,11.25));
#25792=CARTESIAN_POINT('',(3.05801505207583,-53.412531712523,11.5));
#25793=CARTESIAN_POINT('Origin',(0.,0.,11.5));
#25794=CARTESIAN_POINT('',(2.29739178302173,-53.0124970957196,11.0622545443403));
#25795=CARTESIAN_POINT('Ctrl Pts',(2.29739178302173,-53.0124970957196,11.0622545443403));
#25796=CARTESIAN_POINT('Ctrl Pts',(2.67614114119987,-53.2116927560781,11.27766180752));
#25797=CARTESIAN_POINT('Ctrl Pts',(3.05801505207583,-53.412531712523,11.5));
#25798=CARTESIAN_POINT('Ctrl Pts',(2.2079419616008,-52.953989389792,11.));
#25799=CARTESIAN_POINT('Ctrl Pts',(2.2405494369663,-52.9719225189241,11.0192759649605));
#25800=CARTESIAN_POINT('Ctrl Pts',(2.2705255175094,-52.9918321844726,11.0404458048696));
#25801=CARTESIAN_POINT('Ctrl Pts',(2.2973917830217,-53.0124970957195,11.0622545443404));
#25802=CARTESIAN_POINT('Ctrl Pts',(4.51126784227785,-52.8076553394982,11.));
#25803=CARTESIAN_POINT('Ctrl Pts',(4.57608660062692,-52.8996682008571,11.0971961933879));
#25804=CARTESIAN_POINT('Ctrl Pts',(4.64844098161559,-52.9953004405386,11.1987310576087));
#25805=CARTESIAN_POINT('Ctrl Pts',(4.72678212511292,-53.0869825079595,11.2969997378716));
#25806=CARTESIAN_POINT('Origin',(0.,0.,14.5));
#25807=CARTESIAN_POINT('',(3.05801505207583,-53.412531712523,24.2));
#25808=CARTESIAN_POINT('Origin',(0.,0.,24.2));
#25809=CARTESIAN_POINT('',(3.05801505207583,-53.412531712523,14.5));
#25810=CARTESIAN_POINT('Origin',(1.04073669728542,-53.2696785416253,14.5));
#25811=CARTESIAN_POINT('',(1.4061694096632,-53.0436192667856,11.0622545443405));
#25812=CARTESIAN_POINT('',(1.4061694096632,-53.0436192667856,24.2));
#25813=CARTESIAN_POINT('',(1.4061694096632,-53.0436192667856,14.5));
#25814=CARTESIAN_POINT('',(0.675303984907634,-53.495737816465,24.2));
#25815=CARTESIAN_POINT('',(1.27424630420039,-53.1252278380639,24.2));
#25816=CARTESIAN_POINT('',(0.675303984907639,-53.495737816465,11.5));
#25817=CARTESIAN_POINT('',(0.675303984907634,-53.495737816465,14.5));
#25818=CARTESIAN_POINT('Ctrl Pts',(0.675303984907627,-53.495737816465,11.5));
#25819=CARTESIAN_POINT('Ctrl Pts',(0.918332026570836,-53.3453989414732,
11.3527407245756));
#25820=CARTESIAN_POINT('Ctrl Pts',(1.16196424828666,-53.1946863164038,11.2067970124651));
#25821=CARTESIAN_POINT('Ctrl Pts',(1.4061694096632,-53.0436192667856,11.0622545443405));
#25822=CARTESIAN_POINT('Origin',(0.,0.,11.25));
#25823=CARTESIAN_POINT('Ctrl Pts',(1.49132004456263,-52.9790143785696,11.));
#25824=CARTESIAN_POINT('Ctrl Pts',(1.46004329008757,-52.999178187535,11.0192757561174));
#25825=CARTESIAN_POINT('Ctrl Pts',(1.43152846249062,-53.0211308257202,11.0404460254343));
#25826=CARTESIAN_POINT('Ctrl Pts',(1.4061694096632,-53.0436192667856,11.0622545443405));
#25827=CARTESIAN_POINT('Origin',(0.,0.,11.5));
#25828=CARTESIAN_POINT('Origin',(0.,0.,11.25));
#25829=CARTESIAN_POINT('Origin',(0.,0.,11.5));
#25830=CARTESIAN_POINT('Origin',(0.,0.,11.25));
#25831=CARTESIAN_POINT('Origin',(0.,0.,11.5));
#25832=CARTESIAN_POINT('Origin',(0.,0.,14.5));
#25833=CARTESIAN_POINT('Origin',(0.,0.,24.2));
#25834=CARTESIAN_POINT('Origin',(0.,0.,14.5));
#25835=CARTESIAN_POINT('Origin',(0.,0.,24.2));
#25836=CARTESIAN_POINT('Origin',(0.,0.,14.5));
#25837=CARTESIAN_POINT('Origin',(0.,0.,24.2));
#25838=CARTESIAN_POINT('Origin',(0.,0.,14.5));
#25839=CARTESIAN_POINT('Origin',(0.,0.,24.2));
#25840=CARTESIAN_POINT('Origin',(2.67770341754884,-53.2125144041213,14.5));
#25841=CARTESIAN_POINT('',(2.29739178302185,-53.0124970957197,24.2));
#25842=CARTESIAN_POINT('',(2.43468625658986,-53.0847043819776,24.2));
#25843=CARTESIAN_POINT('',(2.29739178302185,-53.0124970957197,14.5));
#25844=CARTESIAN_POINT('Origin',(16.5633108984972,-50.9766292734202,11.25));
#25845=CARTESIAN_POINT('Origin',(16.5633108984972,-50.9766292734202,11.5));
#25846=CARTESIAN_POINT('Origin',(12.9670136041422,-52.0078509283934,11.25));
#25847=CARTESIAN_POINT('Origin',(12.9670136041422,-52.0078509283934,11.5));
#25848=CARTESIAN_POINT('Origin',(9.30754232294745,-52.7856955614544,11.25));
#25849=CARTESIAN_POINT('Origin',(9.30754232294745,-52.7856955614544,11.5));
#25850=CARTESIAN_POINT('Origin',(5.6027256311462,-53.3063735917395,11.25));
#25851=CARTESIAN_POINT('Origin',(5.6027256311462,-53.3063735917395,11.5));
#25852=CARTESIAN_POINT('Origin',(1.87061302325407,-53.5673483282235,11.));
#25853=CARTESIAN_POINT('Origin',(1.87061302325407,-53.5673483282235,24.2));
#25854=CARTESIAN_POINT('Origin',(5.6027256311462,-53.3063735917395,11.));
#25855=CARTESIAN_POINT('Origin',(5.6027256311462,-53.3063735917395,24.2));
#25856=CARTESIAN_POINT('Origin',(9.30754232294745,-52.7856955614544,11.));
#25857=CARTESIAN_POINT('Origin',(9.30754232294745,-52.7856955614544,24.2));
#25858=CARTESIAN_POINT('Origin',(12.9670136041422,-52.0078509283934,11.));
#25859=CARTESIAN_POINT('Origin',(12.9670136041422,-52.0078509283934,24.2));
#25860=CARTESIAN_POINT('Origin',(16.5633108984972,-50.9766292734202,11.));
#25861=CARTESIAN_POINT('Origin',(16.5633108984972,-50.9766292734202,24.2));
#25862=CARTESIAN_POINT('Origin',(36.2555847625696,-39.0419563844501,14.5));
#25863=CARTESIAN_POINT('',(36.2884817614959,-39.0348084727496,11.2969997378715));
#25864=CARTESIAN_POINT('',(36.675489024416,-38.9507189255852,11.5));
#25865=CARTESIAN_POINT('Ctrl Pts',(36.2884817614959,-39.0348084727496,11.2969997378715));
#25866=CARTESIAN_POINT('Ctrl Pts',(36.4816175803015,-38.9928436180799,11.3977655520826));
#25867=CARTESIAN_POINT('Ctrl Pts',(36.675489024416,-38.9507189255852,11.5));
#25868=CARTESIAN_POINT('',(36.675489024416,-38.9507189255852,24.2));
#25869=CARTESIAN_POINT('',(36.675489024416,-38.9507189255852,14.5));
#25870=CARTESIAN_POINT('',(35.8356805007233,-39.1331938433149,24.2));
#25871=CARTESIAN_POINT('',(35.9872681182067,-39.1002566472175,24.2));
#25872=CARTESIAN_POINT('',(35.8356805007233,-39.1331938433149,11.5));
#25873=CARTESIAN_POINT('',(35.8356805007233,-39.1331938433149,14.5));
#25874=CARTESIAN_POINT('Ctrl Pts',(35.8356805007233,-39.1331938433149,11.5));
#25875=CARTESIAN_POINT('Ctrl Pts',(36.0334102765875,-39.0902308064254,11.4654707447276));
#25876=CARTESIAN_POINT('Ctrl Pts',(36.2884817614959,-39.0348084727496,11.2969997378715));
#25877=CARTESIAN_POINT('Origin',(35.8654005008348,-39.8325626455884,11.25));
#25878=CARTESIAN_POINT('',(35.1729694999763,-39.7299015085881,11.5));
#25879=CARTESIAN_POINT('Origin',(35.8654005008348,-39.8325626455884,11.5));
#25880=CARTESIAN_POINT('',(35.027792474811,-40.1699382050837,11.2969997378715));
#25881=CARTESIAN_POINT('Ctrl Pts',(35.027792474811,-40.1699382050837,11.2969997378715));
#25882=CARTESIAN_POINT('Ctrl Pts',(35.1095734294849,-39.922057239828,11.4654707447276));
#25883=CARTESIAN_POINT('Ctrl Pts',(35.1729694999763,-39.7299015085881,11.5));
#25884=CARTESIAN_POINT('Ctrl Pts',(35.027792474811,-40.1699382050837,11.2969997378715));
#25885=CARTESIAN_POINT('Ctrl Pts',(34.9105237912332,-40.1418136232562,11.1987310576086));
#25886=CARTESIAN_POINT('Ctrl Pts',(34.7957766472675,-40.1069743542277,11.0971961933879));
#25887=CARTESIAN_POINT('Ctrl Pts',(34.6892533672809,-40.0706338959167,11.));
#25888=CARTESIAN_POINT('Ctrl Pts',(36.2884817614959,-39.0348084727496,11.2969997378715));
#25889=CARTESIAN_POINT('Ctrl Pts',(36.2727691643543,-38.9152423799721,11.1987310576086));
#25890=CARTESIAN_POINT('Ctrl Pts',(36.2501150911098,-38.7974821376142,11.0971961933879));
#25891=CARTESIAN_POINT('Ctrl Pts',(36.2251084243911,-38.6877437910394,11.));
#25892=CARTESIAN_POINT('Origin',(35.8654005008348,-39.8325626455884,11.));
#25893=CARTESIAN_POINT('',(35.1729694999763,-39.7299015085881,24.2));
#25894=CARTESIAN_POINT('Origin',(35.8654005008348,-39.8325626455884,24.2));
#25895=CARTESIAN_POINT('',(35.1729694999763,-39.7299015085881,14.5));
#25896=CARTESIAN_POINT('Origin',(35.0383399022471,-40.1379685795852,14.5));
#25897=CARTESIAN_POINT('',(34.9037103045179,-40.5460356505823,24.2));
#25898=CARTESIAN_POINT('',(35.1243675165795,-39.8772158387497,24.2));
#25899=CARTESIAN_POINT('',(34.9037103045179,-40.5460356505823,11.5));
#25900=CARTESIAN_POINT('',(34.9037103045179,-40.5460356505823,14.5));
#25901=CARTESIAN_POINT('Ctrl Pts',(34.9037103045179,-40.5460356505823,11.5));
#25902=CARTESIAN_POINT('Ctrl Pts',(34.9658693176641,-40.3576294838963,11.3977655520828));
#25903=CARTESIAN_POINT('Ctrl Pts',(35.027792474811,-40.1699382050837,11.2969997378715));
#25904=CARTESIAN_POINT('Origin',(33.443838774836,-41.4759138875076,14.5));
#25905=CARTESIAN_POINT('',(33.4771542514414,-41.4710781664026,11.2969997378715));
#25906=CARTESIAN_POINT('',(33.8690845744086,-41.4141897191236,11.5));
#25907=CARTESIAN_POINT('Ctrl Pts',(33.4771542514414,-41.4710781664026,11.2969997378715));
#25908=CARTESIAN_POINT('Ctrl Pts',(33.6727469213824,-41.4426880096833,11.3977655520828));
#25909=CARTESIAN_POINT('Ctrl Pts',(33.8690845744086,-41.4141897191236,11.5));
#25910=CARTESIAN_POINT('',(33.8690845744086,-41.4141897191236,24.2));
#25911=CARTESIAN_POINT('',(33.8690845744086,-41.4141897191236,14.5));
#25912=CARTESIAN_POINT('',(33.0185929752635,-41.5376380558916,24.2));
#25913=CARTESIAN_POINT('',(33.1721089155843,-41.5153553108074,24.2));
#25914=CARTESIAN_POINT('',(33.0185929752635,-41.5376380558916,11.5));
#25915=CARTESIAN_POINT('',(33.0185929752635,-41.5376380558916,14.5));
#25916=CARTESIAN_POINT('Ctrl Pts',(33.0185929752635,-41.5376380558916,11.5));
#25917=CARTESIAN_POINT('Ctrl Pts',(33.2188380412863,-41.5085726067192,11.4654707447276));
#25918=CARTESIAN_POINT('Ctrl Pts',(33.4771542514414,-41.4710781664026,11.2969997378715));
#25919=CARTESIAN_POINT('Origin',(32.9994550774553,-42.2373763933203,11.25));
#25920=CARTESIAN_POINT('',(32.3158720826212,-42.0866637887591,11.5));
#25921=CARTESIAN_POINT('Origin',(32.9994550774553,-42.2373763933203,11.5));
#25922=CARTESIAN_POINT('',(32.140353293127,-42.5155015406339,11.2969997378715));
#25923=CARTESIAN_POINT('Ctrl Pts',(32.140353293127,-42.5155015406339,11.2969997378715));
#25924=CARTESIAN_POINT('Ctrl Pts',(32.2392263355501,-42.2739291519686,11.4654707447276));
#25925=CARTESIAN_POINT('Ctrl Pts',(32.3158720826212,-42.0866637887591,11.5));
#25926=CARTESIAN_POINT('Ctrl Pts',(32.140353293127,-42.5155015406339,11.2969997378715));
#25927=CARTESIAN_POINT('Ctrl Pts',(32.0253321418224,-42.4792652190273,11.1987310576086));
#25928=CARTESIAN_POINT('Ctrl Pts',(31.9132947806875,-42.4365064605718,11.0971961933879));
#25929=CARTESIAN_POINT('Ctrl Pts',(31.809565968283,-42.3928238374073,11.));
#25930=CARTESIAN_POINT('Ctrl Pts',(33.4771542514414,-41.4710781664026,11.2969997378715));
#25931=CARTESIAN_POINT('Ctrl Pts',(33.4698204384081,-41.3507072752477,11.1987310576086));
#25932=CARTESIAN_POINT('Ctrl Pts',(33.4554360886017,-41.2316536226561,11.0971961933879));
#25933=CARTESIAN_POINT('Ctrl Pts',(33.4381452969578,-41.1204382162877,11.));
#25934=CARTESIAN_POINT('Origin',(32.9994550774553,-42.2373763933203,11.));
#25935=CARTESIAN_POINT('',(32.3158720826212,-42.0866637887591,24.2));
#25936=CARTESIAN_POINT('Origin',(32.9994550774553,-42.2373763933203,24.2));
#25937=CARTESIAN_POINT('',(32.3158720826212,-42.0866637887591,14.5));
#25938=CARTESIAN_POINT('Origin',(32.1531051159017,-42.4843455428814,14.5));
#25939=CARTESIAN_POINT('',(31.9903381491823,-42.8820272970037,24.2));
#25940=CARTESIAN_POINT('',(32.2571123630091,-42.2302289656376,24.2));
#25941=CARTESIAN_POINT('',(31.9903381491823,-42.8820272970037,11.5));
#25942=CARTESIAN_POINT('',(31.9903381491823,-42.8820272970037,14.5));
#25943=CARTESIAN_POINT('Ctrl Pts',(31.9903381491823,-42.8820272970037,11.5));
#25944=CARTESIAN_POINT('Ctrl Pts',(32.0654882959157,-42.6984160718402,11.3977655520835));
#25945=CARTESIAN_POINT('Ctrl Pts',(32.140353293127,-42.5155015406339,11.2969997378715));
#25946=CARTESIAN_POINT('Origin',(30.4691577663546,-43.7078049072493,14.5));
#25947=CARTESIAN_POINT('',(30.5027294109855,-43.705304935887,11.2969997378715));
#25948=CARTESIAN_POINT('',(30.8976733488635,-43.6758947432898,11.5));
#25949=CARTESIAN_POINT('Ctrl Pts',(30.5027294109855,-43.705304935887,11.2969997378715));
#25950=CARTESIAN_POINT('Ctrl Pts',(30.699826024235,-43.6906277911077,11.3977655520828));
#25951=CARTESIAN_POINT('Ctrl Pts',(30.8976733488635,-43.6758947432898,11.5));
#25952=CARTESIAN_POINT('',(30.8976733488635,-43.6758947432898,24.2));
#25953=CARTESIAN_POINT('',(30.8976733488635,-43.6758947432898,14.5));
#25954=CARTESIAN_POINT('',(30.0406421838458,-43.7397150712088,24.2));
#25955=CARTESIAN_POINT('',(30.195338532774,-43.728195336432,24.2));
#25956=CARTESIAN_POINT('',(30.0406421838458,-43.7397150712088,11.5));
#25957=CARTESIAN_POINT('',(30.0406421838458,-43.7397150712088,14.5));
#25958=CARTESIAN_POINT('Ctrl Pts',(30.0406421838458,-43.7397150712088,11.5));
#25959=CARTESIAN_POINT('Ctrl Pts',(30.242426966194,-43.7246888137001,11.4654707447276));
#25960=CARTESIAN_POINT('Ctrl Pts',(30.5027294109855,-43.705304935887,11.2969997378715));
#25961=CARTESIAN_POINT('Origin',(29.972739626032,-44.4364138889502,11.25));
#25962=CARTESIAN_POINT('',(29.3013349848596,-44.2383840734879,11.5));
#25963=CARTESIAN_POINT('Origin',(29.972739626032,-44.4364138889502,11.5));
#25964=CARTESIAN_POINT('',(29.0963295409359,-44.6539336263215,11.2969997378715));
#25965=CARTESIAN_POINT('Ctrl Pts',(29.0963295409359,-44.6539336263215,11.2969997378715));
#25966=CARTESIAN_POINT('Ctrl Pts',(29.2118129715843,-44.4198467306414,11.4654707447276));
#25967=CARTESIAN_POINT('Ctrl Pts',(29.3013349848596,-44.2383840734879,11.5));
#25968=CARTESIAN_POINT('Ctrl Pts',(29.0963295409359,-44.6539336263215,11.2969997378715));
#25969=CARTESIAN_POINT('Ctrl Pts',(28.9841162933917,-44.609762104652,11.1987310576086));
#25970=CARTESIAN_POINT('Ctrl Pts',(28.875334549849,-44.5592921731428,11.0971961933879));
#25971=CARTESIAN_POINT('Ctrl Pts',(28.774905561374,-44.5084802024738,11.));
#25972=CARTESIAN_POINT('Ctrl Pts',(30.5027294109855,-43.705304935887,11.2969997378715));
#25973=CARTESIAN_POINT('Ctrl Pts',(30.5038101116606,-43.5847156812369,11.1987310576087));
#25974=CARTESIAN_POINT('Ctrl Pts',(30.4977655643985,-43.4649486358399,11.0971961933879));
#25975=CARTESIAN_POINT('Ctrl Pts',(30.4882748868283,-43.3527979999583,11.));
#25976=CARTESIAN_POINT('Origin',(29.972739626032,-44.4364138889502,11.));
#25977=CARTESIAN_POINT('',(29.3013349848596,-44.2383840734879,24.2));
#25978=CARTESIAN_POINT('Origin',(29.972739626032,-44.4364138889502,24.2));
#25979=CARTESIAN_POINT('',(29.3013349848596,-44.2383840734879,14.5));
#25980=CARTESIAN_POINT('Origin',(29.1112236334505,-44.6237430452042,14.5));
#25981=CARTESIAN_POINT('',(28.9211122820414,-45.0091020169205,24.2));
#25982=CARTESIAN_POINT('',(29.2327038004797,-44.3775006619728,24.2));
#25983=CARTESIAN_POINT('',(28.9211122820414,-45.0091020169205,11.5));
#25984=CARTESIAN_POINT('',(28.9211122820413,-45.0091020169205,14.5));
#25985=CARTESIAN_POINT('Ctrl Pts',(28.9211122820414,-45.0091020169205,11.5));
#25986=CARTESIAN_POINT('Ctrl Pts',(29.0088874384019,-44.8311802687101,11.3977655520831));
#25987=CARTESIAN_POINT('Ctrl Pts',(29.0963295409359,-44.6539336263215,11.2969997378715));
#25988=CARTESIAN_POINT('Origin',(27.3460340839842,-45.7267558949762,14.5));
#25989=CARTESIAN_POINT('',(27.379698338963,-45.7266038529658,11.2969997378715));
#25990=CARTESIAN_POINT('',(27.7757317645856,-45.7248151985527,11.5));
#25991=CARTESIAN_POINT('Ctrl Pts',(27.379698338963,-45.7266038529658,11.2969997378715));
#25992=CARTESIAN_POINT('Ctrl Pts',(27.5773386606333,-45.7257112257007,11.397765552083));
#25993=CARTESIAN_POINT('Ctrl Pts',(27.7757317645856,-45.7248151985527,11.5));
#25994=CARTESIAN_POINT('',(27.7757317645856,-45.7248151985527,24.2));
#25995=CARTESIAN_POINT('',(27.7757317645856,-45.7248151985527,14.5));
#25996=CARTESIAN_POINT('',(26.9163364033829,-45.7286965913998,24.2));
#25997=CARTESIAN_POINT('',(27.0714594958567,-45.7279959899203,24.2));
#25998=CARTESIAN_POINT('',(26.9163364033829,-45.7286965913998,11.5));
#25999=CARTESIAN_POINT('',(26.9163364033829,-45.7286965913998,14.5));
#26000=CARTESIAN_POINT('Ctrl Pts',(26.9163364033829,-45.7286965913998,11.5));
#26001=CARTESIAN_POINT('Ctrl Pts',(27.1186778268805,-45.727782731971,11.4654707447276));
#26002=CARTESIAN_POINT('Ctrl Pts',(27.379698338963,-45.7266038529658,11.2969997378715));
#26003=CARTESIAN_POINT('Origin',(26.8,-46.4189616428459,11.25));
#26004=CARTESIAN_POINT('',(26.1440447284116,-46.1745793978374,11.5));
#26005=CARTESIAN_POINT('Origin',(26.8,-46.4189616428459,11.5));
#26006=CARTESIAN_POINT('',(25.9105513959743,-46.5748162359794,11.2969997378715));
#26007=CARTESIAN_POINT('Ctrl Pts',(25.9105513959743,-46.5748162359794,11.2969997378715));
#26008=CARTESIAN_POINT('Ctrl Pts',(26.042082591182,-46.3493552811098,11.4654707447276));
#26009=CARTESIAN_POINT('Ctrl Pts',(26.1440447284116,-46.1745793978374,11.5));
#26010=CARTESIAN_POINT('Ctrl Pts',(25.9105513959743,-46.5748162359794,11.2969997378715));
#26011=CARTESIAN_POINT('Ctrl Pts',(25.8016927438527,-46.5229247134606,11.1987310576087));
#26012=CARTESIAN_POINT('Ctrl Pts',(25.6966965916221,-46.4649894933306,11.0971961933879));
#26013=CARTESIAN_POINT('Ctrl Pts',(25.6000567070134,-46.4072957259707,11.));
#26014=CARTESIAN_POINT('Ctrl Pts',(27.379698338963,-45.7266038529658,11.2969997378715));
#26015=CARTESIAN_POINT('Ctrl Pts',(27.3891882882814,-45.6063837335474,11.1987310576087));
#26016=CARTESIAN_POINT('Ctrl Pts',(27.3915129919902,-45.4864867883511,11.0971961933879));
#26017=CARTESIAN_POINT('Ctrl Pts',(27.3898686661209,-45.3739473095812,11.));
#26018=CARTESIAN_POINT('Origin',(26.8,-46.4189616428459,11.));
#26019=CARTESIAN_POINT('',(26.1440447284116,-46.1745793978374,24.2));
#26020=CARTESIAN_POINT('Origin',(26.8,-46.4189616428459,24.2));
#26021=CARTESIAN_POINT('',(26.1440447284116,-46.1745793978374,14.5));
#26022=CARTESIAN_POINT('Origin',(25.9275151957071,-46.5457381569736,14.5));
#26023=CARTESIAN_POINT('',(25.7109856630026,-46.9168969161098,24.2));
#26024=CARTESIAN_POINT('',(26.0658764434955,-46.3085696358935,24.2));
#26025=CARTESIAN_POINT('',(25.7109856630026,-46.9168969161098,11.5));
#26026=CARTESIAN_POINT('',(25.7109856630026,-46.9168969161098,14.5));
#26027=CARTESIAN_POINT('Ctrl Pts',(25.7109856630026,-46.9168969161098,11.5));
#26028=CARTESIAN_POINT('Ctrl Pts',(25.8109581972526,-46.7455314617236,11.3977655520818));
#26029=CARTESIAN_POINT('Ctrl Pts',(25.9105513959743,-46.5748162359794,11.2969997378715));
#26030=CARTESIAN_POINT('Origin',(24.0896832723706,-47.5229307244202,14.5));
#26031=CARTESIAN_POINT('',(24.1232761288306,-47.525127352495,11.2969997378715));
#26032=CARTESIAN_POINT('',(24.5184696071576,-47.5509689504103,11.5));
#26033=CARTESIAN_POINT('Ctrl Pts',(24.1232761288306,-47.525127352495,11.2969997378715));
#26034=CARTESIAN_POINT('Ctrl Pts',(24.3204972751414,-47.5380235915345,11.3977655520831));
#26035=CARTESIAN_POINT('Ctrl Pts',(24.5184696071576,-47.5509689504103,11.5));
#26036=CARTESIAN_POINT('',(24.5184696071576,-47.5509689504103,24.2));
#26037=CARTESIAN_POINT('',(24.5184696071576,-47.5509689504103,14.5));
#26038=CARTESIAN_POINT('',(23.6608969375836,-47.49489249843,24.2));
#26039=CARTESIAN_POINT('',(23.8156910294893,-47.5050144435077,24.2));
#26040=CARTESIAN_POINT('',(23.6608969375836,-47.49489249843,11.5));
#26041=CARTESIAN_POINT('',(23.6608969375836,-47.49489249843,14.5));
#26042=CARTESIAN_POINT('Ctrl Pts',(23.6608969375836,-47.49489249843,11.5));
#26043=CARTESIAN_POINT('Ctrl Pts',(23.8628092151544,-47.5080954893125,11.4654707447276));
#26044=CARTESIAN_POINT('Ctrl Pts',(24.1232761288306,-47.525127352495,11.2969997378715));
#26045=CARTESIAN_POINT('Origin',(23.4966934678945,-48.1753608816354,11.25));
#26046=CARTESIAN_POINT('',(22.859383314037,-47.8858168128132,11.5));
#26047=CARTESIAN_POINT('Origin',(23.4966934678945,-48.1753608816354,11.5));
#26048=CARTESIAN_POINT('',(22.5985396491308,-48.2687910226197,11.2969997378715));
#26049=CARTESIAN_POINT('Ctrl Pts',(22.5985396491308,-48.2687910226197,11.2969997378715));
#26050=CARTESIAN_POINT('Ctrl Pts',(22.7454778021365,-48.0530544316696,11.4654707447276));
#26051=CARTESIAN_POINT('Ctrl Pts',(22.859383314037,-47.8858168128132,11.5));
#26052=CARTESIAN_POINT('Ctrl Pts',(22.5985396491308,-48.2687910226197,11.2969997378715));
#26053=CARTESIAN_POINT('Ctrl Pts',(22.4935659408428,-48.2094323095332,11.1987310576086));
#26054=CARTESIAN_POINT('Ctrl Pts',(22.3928669106238,-48.1443140553513,11.0971961933879));
#26055=CARTESIAN_POINT('Ctrl Pts',(22.300486949685,-48.0800195695356,11.));
#26056=CARTESIAN_POINT('Ctrl Pts',(24.1232761288306,-47.525127352495,11.2969997378715));
#26057=CARTESIAN_POINT('Ctrl Pts',(24.1411290927132,-47.4058620686457,11.1987310576087));
#26058=CARTESIAN_POINT('Ctrl Pts',(24.1518117216703,-47.2864193495151,11.0971961933879));
#26059=CARTESIAN_POINT('Ctrl Pts',(24.1580217584921,-47.174039308885,11.));
#26060=CARTESIAN_POINT('Origin',(23.4966934678945,-48.1753608816354,11.));
#26061=CARTESIAN_POINT('',(22.859383314037,-47.8858168128132,24.2));
#26062=CARTESIAN_POINT('Origin',(23.4966934678945,-48.1753608816354,24.2));
#26063=CARTESIAN_POINT('',(22.859383314037,-47.8858168128132,14.5));
#26064=CARTESIAN_POINT('Origin',(20.7159699453406,-49.087578612363,14.5));
#26065=CARTESIAN_POINT('',(20.2901839602893,-49.0296980633778,11.0622545443403));
#26066=CARTESIAN_POINT('',(21.1417559303918,-49.1454591613482,11.5));
#26067=CARTESIAN_POINT('Ctrl Pts',(20.2901839602893,-49.0296980633778,11.0622545443403));
#26068=CARTESIAN_POINT('Ctrl Pts',(20.7142208656047,-49.0873408457411,11.2776618075212));
#26069=CARTESIAN_POINT('Ctrl Pts',(21.1417559303918,-49.1454591613482,11.5));
#26070=CARTESIAN_POINT('',(21.1417559303918,-49.1454591613482,24.2));
#26071=CARTESIAN_POINT('',(21.1417559303918,-49.1454591613482,14.5));
#26072=CARTESIAN_POINT('',(20.2901839602894,-49.0296980633778,24.2));
#26073=CARTESIAN_POINT('',(20.4438949103711,-49.0505932419138,24.2));
#26074=CARTESIAN_POINT('',(20.2901839602894,-49.0296980633778,14.5));
#26075=CARTESIAN_POINT('Origin',(0.,0.,14.5));
#26076=CARTESIAN_POINT('',(22.3755977062724,-48.5961174095941,11.5));
#26077=CARTESIAN_POINT('Origin',(0.,0.,11.5));
#26078=CARTESIAN_POINT('',(22.3755977062724,-48.5961174095941,24.2));
#26079=CARTESIAN_POINT('',(22.3755977062724,-48.5961174095941,14.5));
#26080=CARTESIAN_POINT('Origin',(0.,0.,24.2));
#26081=CARTESIAN_POINT('Origin',(0.,0.,11.25));
#26082=CARTESIAN_POINT('Ctrl Pts',(20.1861178092024,-49.0053124446014,11.));
#26083=CARTESIAN_POINT('Ctrl Pts',(20.2228923045819,-49.0110116603164,11.0192759649605));
#26084=CARTESIAN_POINT('Ctrl Pts',(20.2578701129328,-49.019468202751,11.0404458048696));
#26085=CARTESIAN_POINT('Ctrl Pts',(20.2901839602893,-49.0296980633778,11.0622545443404));
#26086=CARTESIAN_POINT('Ctrl Pts',(22.3755977062724,-48.5961174095941,11.5));
#26087=CARTESIAN_POINT('Ctrl Pts',(22.4872805622719,-48.4321431243045,11.397765552083));
#26088=CARTESIAN_POINT('Ctrl Pts',(22.5985396491308,-48.2687910226197,11.2969997378715));
#26089=CARTESIAN_POINT('Origin',(22.6174905101547,-48.2409671112037,14.5));
#26090=CARTESIAN_POINT('',(22.7720587566113,-48.0140279134694,24.2));
#26091=CARTESIAN_POINT('Origin',(46.653263217121,-25.7335348523128,14.5));
#26092=CARTESIAN_POINT('',(46.6663199357044,-26.1630385020257,24.2));
#26093=CARTESIAN_POINT('',(46.6402064985376,-25.3040312025999,24.2));
#26094=CARTESIAN_POINT('',(46.6449200416998,-25.459084248916,24.2));
#26095=CARTESIAN_POINT('',(46.6663199357044,-26.1630385020257,11.5));
#26096=CARTESIAN_POINT('',(46.6663199357044,-26.1630385020257,14.5));
#26097=CARTESIAN_POINT('',(46.6402064985376,-25.3040312025998,11.0622545443403));
#26098=CARTESIAN_POINT('Ctrl Pts',(46.6663199357044,-26.1630385020257,11.5));
#26099=CARTESIAN_POINT('Ctrl Pts',(46.6532095816264,-25.7317705008368,11.2776618075201));
#26100=CARTESIAN_POINT('Ctrl Pts',(46.6402064985376,-25.3040312025998,11.0622545443403));
#26101=CARTESIAN_POINT('',(46.6402064985376,-25.3040312025999,14.5));
#26102=CARTESIAN_POINT('Origin',(0.,0.,11.25));
#26103=CARTESIAN_POINT('',(45.9910159507966,-27.3326993144397,11.5));
#26104=CARTESIAN_POINT('Origin',(0.,0.,11.5));
#26105=CARTESIAN_POINT('',(45.6421789133341,-27.5202050337907,11.2969997378715));
#26106=CARTESIAN_POINT('Ctrl Pts',(45.6421789133341,-27.5202050337907,11.2969997378715));
#26107=CARTESIAN_POINT('Ctrl Pts',(45.8162658964866,-27.4266303800122,11.3977655520824));
#26108=CARTESIAN_POINT('Ctrl Pts',(45.9910159507966,-27.3326993144397,11.5));
#26109=CARTESIAN_POINT('Ctrl Pts',(45.6421789133341,-27.5202050337907,11.2969997378715));
#26110=CARTESIAN_POINT('Ctrl Pts',(45.5941181138995,-27.4096017073998,11.1987310576087));
#26111=CARTESIAN_POINT('Ctrl Pts',(45.5398824992088,-27.3026476059644,11.097196193388));
#26112=CARTESIAN_POINT('Ctrl Pts',(45.4855965606673,-27.2040531083184,11.));
#26113=CARTESIAN_POINT('Ctrl Pts',(46.6402064985376,-25.3040312025997,11.0622545443404));
#26114=CARTESIAN_POINT('Ctrl Pts',(46.6334103949641,-25.2708250622694,11.0404458048696));
#26115=CARTESIAN_POINT('Ctrl Pts',(46.6286563549092,-25.2351549166271,11.0192759649605));
#26116=CARTESIAN_POINT('Ctrl Pts',(46.6268323415836,-25.1979861455206,11.));
#26117=CARTESIAN_POINT('Origin',(0.,0.,14.5));
#26118=CARTESIAN_POINT('',(45.9910159507966,-27.3326993144397,24.2));
#26119=CARTESIAN_POINT('Origin',(0.,0.,24.2));
#26120=CARTESIAN_POINT('',(45.9910159507966,-27.3326993144397,14.5));
#26121=CARTESIAN_POINT('Origin',(45.6125265198355,-27.5361436893127,14.5));
#26122=CARTESIAN_POINT('',(45.2340370888743,-27.7395880641857,24.2));
#26123=CARTESIAN_POINT('',(45.3706737374994,-27.666143589148,24.2));
#26124=CARTESIAN_POINT('',(45.2340370888743,-27.7395880641857,11.5));
#26125=CARTESIAN_POINT('',(45.2340370888743,-27.7395880641857,14.5));
#26126=CARTESIAN_POINT('Ctrl Pts',(45.2340370888743,-27.7395880641857,11.5));
#26127=CARTESIAN_POINT('Ctrl Pts',(45.412264930673,-27.6437876298972,11.4654707447276));
#26128=CARTESIAN_POINT('Ctrl Pts',(45.6421789133341,-27.5202050337907,11.2969997378715));
#26129=CARTESIAN_POINT('Origin',(44.74453756444,-28.9252163854584,14.5));
#26130=CARTESIAN_POINT('',(44.727601817449,-29.3545845765144,24.2));
#26131=CARTESIAN_POINT('',(44.7614733114311,-28.4958481944024,24.2));
#26132=CARTESIAN_POINT('',(44.7553594188847,-28.6508523394404,24.2));
#26133=CARTESIAN_POINT('',(44.727601817449,-29.3545845765144,11.5));
#26134=CARTESIAN_POINT('',(44.727601817449,-29.3545845765144,14.5));
#26135=CARTESIAN_POINT('',(44.7432107494939,-28.9588548268927,11.2969997378715));
#26136=CARTESIAN_POINT('Ctrl Pts',(44.727601817449,-29.3545845765144,11.5));
#26137=CARTESIAN_POINT('Ctrl Pts',(44.7354211182388,-29.156343599178,11.3977655520834));
#26138=CARTESIAN_POINT('Ctrl Pts',(44.7432107494939,-28.9588548268927,11.2969997378715));
#26139=CARTESIAN_POINT('',(44.7614733114311,-28.4958481944024,11.5));
#26140=CARTESIAN_POINT('Ctrl Pts',(44.7432107494939,-28.9588548268927,11.2969997378715));
#26141=CARTESIAN_POINT('Ctrl Pts',(44.7534983948587,-28.6980344637377,11.4654707447276));
#26142=CARTESIAN_POINT('Ctrl Pts',(44.7614733114311,-28.4958481944024,11.5));
#26143=CARTESIAN_POINT('',(44.7614733114311,-28.4958481944024,14.5));
#26144=CARTESIAN_POINT('Origin',(0.,0.,11.25));
#26145=CARTESIAN_POINT('',(43.9723514253573,-30.4742893292835,11.5));
#26146=CARTESIAN_POINT('Origin',(0.,0.,11.5));
#26147=CARTESIAN_POINT('',(43.6112843995965,-30.6370046524816,11.2969997378715));
#26148=CARTESIAN_POINT('Ctrl Pts',(43.6112843995965,-30.6370046524816,11.2969997378715));
#26149=CARTESIAN_POINT('Ctrl Pts',(43.7914747534875,-30.5558016359259,11.3977655520825));
#26150=CARTESIAN_POINT('Ctrl Pts',(43.9723514253573,-30.4742893292835,11.5));
#26151=CARTESIAN_POINT('Ctrl Pts',(43.6112843995965,-30.6370046524816,11.2969997378715));
#26152=CARTESIAN_POINT('Ctrl Pts',(43.5710559718872,-30.523318198341,11.1987310576086));
#26153=CARTESIAN_POINT('Ctrl Pts',(43.5244132133966,-30.412841346489,11.0971961933879));
#26154=CARTESIAN_POINT('Ctrl Pts',(43.4771371171594,-30.3107002244375,11.));
#26155=CARTESIAN_POINT('Ctrl Pts',(44.7432107494939,-28.9588548268927,11.2969997378715));
#26156=CARTESIAN_POINT('Ctrl Pts',(44.6227326704691,-28.9641433735292,11.1987310576086));
#26157=CARTESIAN_POINT('Ctrl Pts',(44.5028276322628,-28.9622823180478,11.0971961933879));
#26158=CARTESIAN_POINT('Ctrl Pts',(44.390414095648,-28.9567114226892,11.));
#26159=CARTESIAN_POINT('Origin',(0.,0.,14.5));
#26160=CARTESIAN_POINT('',(43.9723514253573,-30.4742893292835,24.2));
#26161=CARTESIAN_POINT('Origin',(0.,0.,24.2));
#26162=CARTESIAN_POINT('',(43.9723514253573,-30.4742893292835,14.5));
#26163=CARTESIAN_POINT('Origin',(43.5805924134329,-30.6508360358313,14.5));
#26164=CARTESIAN_POINT('',(43.1888334015085,-30.827382742379,24.2));
#26165=CARTESIAN_POINT('',(43.3302604377194,-30.7636484651835,24.2));
#26166=CARTESIAN_POINT('',(43.1888334015085,-30.827382742379,11.5));
#26167=CARTESIAN_POINT('',(43.1888334015085,-30.827382742379,14.5));
#26168=CARTESIAN_POINT('Ctrl Pts',(43.1888334015085,-30.827382742379,11.5));
#26169=CARTESIAN_POINT('Ctrl Pts',(43.3733097897213,-30.7442482189004,11.4654707447276));
#26170=CARTESIAN_POINT('Ctrl Pts',(43.6112843995965,-30.6370046524816,11.2969997378715));
#26171=CARTESIAN_POINT('Origin',(42.6178210224503,-31.9759771719266,14.5));
#26172=CARTESIAN_POINT('',(42.5709753191417,-32.4031180656588,24.2));
#26173=CARTESIAN_POINT('',(42.6646667257588,-31.5488362781943,24.2));
#26174=CARTESIAN_POINT('',(42.6477551837738,-31.7030363573407,24.2));
#26175=CARTESIAN_POINT('',(42.5709753191417,-32.4031180656588,11.5));
#26176=CARTESIAN_POINT('',(42.5709753191417,-32.4031180656588,14.5));
#26177=CARTESIAN_POINT('',(42.6141509405019,-32.0094411178763,11.2969997378715));
#26178=CARTESIAN_POINT('Ctrl Pts',(42.5709753191417,-32.4031180656588,11.5));
#26179=CARTESIAN_POINT('Ctrl Pts',(42.5926041640384,-32.2059054402292,11.3977655520831));
#26180=CARTESIAN_POINT('Ctrl Pts',(42.6141509405019,-32.0094411178763,11.2969997378715));
#26181=CARTESIAN_POINT('',(42.6646667257588,-31.5488362781943,11.5));
#26182=CARTESIAN_POINT('Ctrl Pts',(42.6141509405019,-32.0094411178763,11.2969997378715));
#26183=CARTESIAN_POINT('Ctrl Pts',(42.642607434494,-31.7499737298809,11.4654707447276));
#26184=CARTESIAN_POINT('Ctrl Pts',(42.6646667257588,-31.5488362781943,11.5));
#26185=CARTESIAN_POINT('',(42.6646667257588,-31.5488362781943,14.5));
#26186=CARTESIAN_POINT('Origin',(0.,0.,11.25));
#26187=CARTESIAN_POINT('',(41.7394580238585,-33.4674116697804,11.5));
#26188=CARTESIAN_POINT('Origin',(0.,0.,11.5));
#26189=CARTESIAN_POINT('',(41.3679200920551,-33.6045438641268,11.2969997378715));
#26190=CARTESIAN_POINT('Ctrl Pts',(41.3679200920551,-33.6045438641268,11.2969997378715));
#26191=CARTESIAN_POINT('Ctrl Pts',(41.5533359473939,-33.5361080977279,11.3977655520833));
#26192=CARTESIAN_POINT('Ctrl Pts',(41.7394580238585,-33.4674116697804,11.5));
#26193=CARTESIAN_POINT('Ctrl Pts',(41.3679200920551,-33.6045438641268,11.2969997378715));
#26194=CARTESIAN_POINT('Ctrl Pts',(41.3357200249272,-33.4883281512133,11.1987310576087));
#26195=CARTESIAN_POINT('Ctrl Pts',(41.2968973614675,-33.3748667810618,11.0971961933879));
#26196=CARTESIAN_POINT('Ctrl Pts',(41.2568614319233,-33.2696766558842,11.));
#26197=CARTESIAN_POINT('Ctrl Pts',(42.6141509405019,-32.0094411178763,11.2969997378715));
#26198=CARTESIAN_POINT('Ctrl Pts',(42.4935974296578,-32.0063126559227,11.1987310576086));
#26199=CARTESIAN_POINT('Ctrl Pts',(42.3741142947661,-31.9960919812296,11.0971961933879));
#26200=CARTESIAN_POINT('Ctrl Pts',(42.2623631978924,-31.9826930843766,11.));
#26201=CARTESIAN_POINT('Origin',(0.,0.,14.5));
#26202=CARTESIAN_POINT('',(41.7394580238585,-33.4674116697804,24.2));
#26203=CARTESIAN_POINT('Origin',(0.,0.,24.2));
#26204=CARTESIAN_POINT('',(41.7394580238585,-33.4674116697804,14.5));
#26205=CARTESIAN_POINT('Origin',(41.3363380414975,-33.6162005901948,14.5));
#26206=CARTESIAN_POINT('',(40.9332180591366,-33.7649895106092,24.2));
#26207=CARTESIAN_POINT('',(41.0787464646293,-33.7112759382477,24.2));
#26208=CARTESIAN_POINT('',(40.9332180591366,-33.7649895106092,11.5));
#26209=CARTESIAN_POINT('',(40.9332180591366,-33.7649895106092,14.5));
#26210=CARTESIAN_POINT('Ctrl Pts',(40.9332180591366,-33.7649895106092,11.5));
#26211=CARTESIAN_POINT('Ctrl Pts',(41.1230442433438,-33.6949259209822,11.4654707447276));
#26212=CARTESIAN_POINT('Ctrl Pts',(41.3679200920551,-33.6045438641268,11.2969997378715));
#26213=CARTESIAN_POINT('Origin',(40.2834747403676,-34.870954211827,14.5));
#26214=CARTESIAN_POINT('',(40.2069473082993,-35.2937868207372,24.2));
#26215=CARTESIAN_POINT('',(40.3600021724359,-34.4481216029168,24.2));
#26216=CARTESIAN_POINT('',(40.332375372345,-34.600766368886,24.2));
#26217=CARTESIAN_POINT('',(40.2069473082993,-35.2937868207372,11.5));
#26218=CARTESIAN_POINT('',(40.2069473082993,-35.2937868207372,14.5));
#26219=CARTESIAN_POINT('',(40.2774792716874,-34.9040806293114,11.2969997378715));
#26220=CARTESIAN_POINT('Ctrl Pts',(40.2069473082993,-35.2937868207372,11.5));
#26221=CARTESIAN_POINT('Ctrl Pts',(40.2422803237448,-35.0985633473018,11.3977655520828));
#26222=CARTESIAN_POINT('Ctrl Pts',(40.2774792716874,-34.9040806293114,11.2969997378715));
#26223=CARTESIAN_POINT('',(40.3600021724359,-34.4481216029168,11.5));
#26224=CARTESIAN_POINT('Ctrl Pts',(40.2774792716874,-34.9040806293114,11.2969997378715));
#26225=CARTESIAN_POINT('Ctrl Pts',(40.3239659771285,-34.6472303155083,11.4654707447276));
#26226=CARTESIAN_POINT('Ctrl Pts',(40.3600021724359,-34.4481216029168,11.5));
#26227=CARTESIAN_POINT('',(40.3600021724359,-34.4481216029168,14.5));
#26228=CARTESIAN_POINT('Origin',(0.,0.,11.25));
#26229=CARTESIAN_POINT('',(39.3032141785033,-36.2974841447544,11.5));
#26230=CARTESIAN_POINT('Origin',(0.,0.,11.5));
#26231=CARTESIAN_POINT('',(38.4781801929733,-36.5380966439885,11.0622545443402));
#26232=CARTESIAN_POINT('Ctrl Pts',(38.4781801929733,-36.5380966439885,11.0622545443402));
#26233=CARTESIAN_POINT('Ctrl Pts',(38.8890026134927,-36.4182845985743,11.277661807521));
#26234=CARTESIAN_POINT('Ctrl Pts',(39.3032141785033,-36.2974841447544,11.5));
#26235=CARTESIAN_POINT('Ctrl Pts',(38.3731925086332,-36.5581467896744,11.));
#26236=CARTESIAN_POINT('Ctrl Pts',(38.4091057617122,-36.5483957475015,11.0192759649605));
#26237=CARTESIAN_POINT('Ctrl Pts',(38.4444991653313,-36.5418944270792,11.0404458048696));
#26238=CARTESIAN_POINT('Ctrl Pts',(38.4781801929732,-36.5380966439885,11.0622545443403));
#26239=CARTESIAN_POINT('Ctrl Pts',(40.2774792716874,-34.9040806293114,11.2969997378715));
#26240=CARTESIAN_POINT('Ctrl Pts',(40.1574376536108,-34.8925504003199,11.1987310576087));
#26241=CARTESIAN_POINT('Ctrl Pts',(40.0389585318564,-34.8740199005147,11.0971961933879));
#26242=CARTESIAN_POINT('Ctrl Pts',(39.9284143148345,-34.8528582802461,11.));
#26243=CARTESIAN_POINT('Origin',(0.,0.,14.5));
#26244=CARTESIAN_POINT('',(39.3032141785033,-36.2974841447544,24.2));
#26245=CARTESIAN_POINT('Origin',(0.,0.,24.2));
#26246=CARTESIAN_POINT('',(39.3032141785033,-36.2974841447544,14.5));
#26247=CARTESIAN_POINT('Origin',(37.7528714186304,-37.5960434680237,14.5));
#26248=CARTESIAN_POINT('',(37.8587077455022,-37.1795791419031,11.0622545443405));
#26249=CARTESIAN_POINT('',(37.8587077455022,-37.1795791419031,24.2));
#26250=CARTESIAN_POINT('',(37.8587077455022,-37.1795791419031,14.5));
#26251=CARTESIAN_POINT('',(37.6470350917587,-38.0125077941444,24.2));
#26252=CARTESIAN_POINT('',(37.8205002822982,-37.3299249247391,24.2));
#26253=CARTESIAN_POINT('',(37.6470350917587,-38.0125077941444,11.5));
#26254=CARTESIAN_POINT('',(37.6470350917587,-38.0125077941444,14.5));
#26255=CARTESIAN_POINT('Ctrl Pts',(37.6470350917587,-38.0125077941444,11.5));
#26256=CARTESIAN_POINT('Ctrl Pts',(37.7174206768073,-37.7355415944255,11.3527407245747));
#26257=CARTESIAN_POINT('Ctrl Pts',(37.787981243994,-37.4578868426719,11.2067970124647));
#26258=CARTESIAN_POINT('Ctrl Pts',(37.8587077455022,-37.1795791419031,11.0622545443405));
#26259=CARTESIAN_POINT('Origin',(0.,0.,11.25));
#26260=CARTESIAN_POINT('Ctrl Pts',(37.8750816598376,-37.0739556732301,11.));
#26261=CARTESIAN_POINT('Ctrl Pts',(37.8665900041964,-37.1101869628422,11.0192757561174));
#26262=CARTESIAN_POINT('Ctrl Pts',(37.8613277376751,-37.1457864328837,11.0404460254343));
#26263=CARTESIAN_POINT('Ctrl Pts',(37.8587077455022,-37.1795791419031,11.0622545443405));
#26264=CARTESIAN_POINT('Origin',(0.,0.,11.5));
#26265=CARTESIAN_POINT('Origin',(0.,0.,11.25));
#26266=CARTESIAN_POINT('Origin',(0.,0.,11.5));
#26267=CARTESIAN_POINT('Origin',(0.,0.,11.25));
#26268=CARTESIAN_POINT('Origin',(0.,0.,11.5));
#26269=CARTESIAN_POINT('Origin',(0.,0.,11.25));
#26270=CARTESIAN_POINT('Origin',(0.,0.,11.5));
#26271=CARTESIAN_POINT('Origin',(0.,0.,11.25));
#26272=CARTESIAN_POINT('Origin',(0.,0.,11.5));
#26273=CARTESIAN_POINT('Origin',(0.,0.,14.5));
#26274=CARTESIAN_POINT('Origin',(0.,0.,24.2));
#26275=CARTESIAN_POINT('Origin',(0.,0.,14.5));
#26276=CARTESIAN_POINT('Origin',(0.,0.,24.2));
#26277=CARTESIAN_POINT('Origin',(0.,0.,14.5));
#26278=CARTESIAN_POINT('Origin',(0.,0.,24.2));
#26279=CARTESIAN_POINT('Origin',(0.,0.,14.5));
#26280=CARTESIAN_POINT('Origin',(0.,0.,24.2));
#26281=CARTESIAN_POINT('Origin',(0.,0.,14.5));
#26282=CARTESIAN_POINT('Origin',(0.,0.,24.2));
#26283=CARTESIAN_POINT('Origin',(38.8906971857384,-36.4177903943714,14.5));
#26284=CARTESIAN_POINT('',(38.4781801929734,-36.5380966439885,24.2));
#26285=CARTESIAN_POINT('',(38.6271009679847,-36.4946654635865,24.2));
#26286=CARTESIAN_POINT('',(38.4781801929734,-36.5380966439885,14.5));
#26287=CARTESIAN_POINT('Origin',(45.4553779539844,-28.4036725628998,11.25));
#26288=CARTESIAN_POINT('Origin',(45.4553779539844,-28.4036725628998,11.5));
#26289=CARTESIAN_POINT('Origin',(43.3633108984972,-31.5052895228766,11.25));
#26290=CARTESIAN_POINT('Origin',(43.3633108984972,-31.5052895228766,11.5));
#26291=CARTESIAN_POINT('Origin',(41.0599821511772,-34.4534158791985,11.25));
#26292=CARTESIAN_POINT('Origin',(41.0599821511772,-34.4534158791985,11.5));
#26293=CARTESIAN_POINT('Origin',(38.5566132981517,-37.2336886566023,11.));
#26294=CARTESIAN_POINT('Origin',(38.5566132981517,-37.2336886566023,24.2));
#26295=CARTESIAN_POINT('Origin',(41.0599821511772,-34.4534158791985,11.));
#26296=CARTESIAN_POINT('Origin',(41.0599821511772,-34.4534158791985,24.2));
#26297=CARTESIAN_POINT('Origin',(43.3633108984972,-31.5052895228766,11.));
#26298=CARTESIAN_POINT('Origin',(43.3633108984972,-31.5052895228766,24.2));
#26299=CARTESIAN_POINT('Origin',(45.4553779539844,-28.4036725628998,11.));
#26300=CARTESIAN_POINT('Origin',(45.4553779539844,-28.4036725628998,24.2));
#26301=CARTESIAN_POINT('Origin',(53.2009069058212,-2.89918767921613,14.5));
#26302=CARTESIAN_POINT('',(53.2196056697667,-2.87119372617343,11.2969997378715));
#26303=CARTESIAN_POINT('',(53.4395818891992,-2.54186693349002,11.5));
#26304=CARTESIAN_POINT('Ctrl Pts',(53.2196056697666,-2.87119372617343,11.2969997378715));
#26305=CARTESIAN_POINT('Ctrl Pts',(53.3293847135435,-2.70684332282478,11.397765552083));
#26306=CARTESIAN_POINT('Ctrl Pts',(53.4395818891992,-2.54186693349002,11.5));
#26307=CARTESIAN_POINT('',(53.4395818891992,-2.54186693349002,24.2));
#26308=CARTESIAN_POINT('',(53.4395818891992,-2.54186693349002,14.5));
#26309=CARTESIAN_POINT('',(52.9622319224431,-3.25650842494224,24.2));
#26310=CARTESIAN_POINT('',(53.048394829969,-3.127513781535,24.2));
#26311=CARTESIAN_POINT('',(52.9622319224431,-3.25650842494224,11.5));
#26312=CARTESIAN_POINT('',(52.9622319224431,-3.25650842494223,14.5));
#26313=CARTESIAN_POINT('Ctrl Pts',(52.9622319224431,-3.25650842494224,11.5));
#26314=CARTESIAN_POINT('Ctrl Pts',(53.0746221867387,-3.08824875867116,11.4654707447276));
#26315=CARTESIAN_POINT('Ctrl Pts',(53.2196056697667,-2.87119372617343,11.2969997378715));
#26316=CARTESIAN_POINT('Origin',(53.4694330939266,-3.73894699268513,11.25));
#26317=CARTESIAN_POINT('',(52.9000254978827,-4.14610174160441,11.5));
#26318=CARTESIAN_POINT('Origin',(53.4694330939266,-3.73894699268513,11.5));
#26319=CARTESIAN_POINT('',(53.1012690601164,-4.56348608673266,11.2969997378715));
#26320=CARTESIAN_POINT('Ctrl Pts',(53.1012690601164,-4.56348608673266,11.2969997378715));
#26321=CARTESIAN_POINT('Ctrl Pts',(52.9879047683306,-4.32836561796952,11.4654707447276));
#26322=CARTESIAN_POINT('Ctrl Pts',(52.9000254978827,-4.14610174160441,11.5));
#26323=CARTESIAN_POINT('Ctrl Pts',(52.7887618365133,-4.72722156957732,11.));
#26324=CARTESIAN_POINT('Ctrl Pts',(52.8906324750224,-4.67936541951144,11.0971961933879));
#26325=CARTESIAN_POINT('Ctrl Pts',(52.9973760525035,-4.6247166282963,11.1987310576087));
#26326=CARTESIAN_POINT('Ctrl Pts',(53.1012690601164,-4.56348608673266,11.2969997378715));
#26327=CARTESIAN_POINT('Ctrl Pts',(53.2196056697666,-2.87119372617344,11.2969997378715));
#26328=CARTESIAN_POINT('Ctrl Pts',(53.1252453861049,-2.79609996399364,11.1987310576087));
#26329=CARTESIAN_POINT('Ctrl Pts',(53.0271462715192,-2.72712717637234,11.0971961933879));
#26330=CARTESIAN_POINT('Ctrl Pts',(52.9329273198661,-2.66555910641112,11.));
#26331=CARTESIAN_POINT('Origin',(53.4694330939266,-3.73894699268513,11.));
#26332=CARTESIAN_POINT('',(52.9000254978827,-4.14610174160441,24.2));
#26333=CARTESIAN_POINT('Origin',(53.4694330939266,-3.73894699268513,24.2));
#26334=CARTESIAN_POINT('',(52.9000254978827,-4.14610174160441,14.5));
#26335=CARTESIAN_POINT('Origin',(53.0866482765093,-4.53316220395422,14.5));
#26336=CARTESIAN_POINT('',(53.273271055136,-4.92022266630402,24.2));
#26337=CARTESIAN_POINT('',(52.9673972893853,-4.28583257703742,24.2));
#26338=CARTESIAN_POINT('',(53.273271055136,-4.92022266630402,11.5));
#26339=CARTESIAN_POINT('',(53.273271055136,-4.92022266630402,14.5));
#26340=CARTESIAN_POINT('Ctrl Pts',(53.273271055136,-4.92022266630402,11.5));
#26341=CARTESIAN_POINT('Ctrl Pts',(53.1871065865071,-4.74151533319572,11.3977655520826));
#26342=CARTESIAN_POINT('Ctrl Pts',(53.1012690601164,-4.56348608673266,11.2969997378715));
#26343=CARTESIAN_POINT('Origin',(0.,0.,11.25));
#26344=CARTESIAN_POINT('',(53.1320940795741,-6.26343186434448,11.5));
#26345=CARTESIAN_POINT('Origin',(0.,0.,11.5));
#26346=CARTESIAN_POINT('',(52.889681035389,-6.5766116681379,11.2969997378715));
#26347=CARTESIAN_POINT('Ctrl Pts',(52.889681035389,-6.5766116681379,11.2969997378715));
#26348=CARTESIAN_POINT('Ctrl Pts',(53.0106571675296,-6.42031941309508,11.3977655520838));
#26349=CARTESIAN_POINT('Ctrl Pts',(53.1320940795741,-6.26343186434448,11.5));
#26350=CARTESIAN_POINT('Ctrl Pts',(52.889681035389,-6.5766116681379,11.2969997378715));
#26351=CARTESIAN_POINT('Ctrl Pts',(52.8007888846856,-6.49511858993886,11.1987310576086));
#26352=CARTESIAN_POINT('Ctrl Pts',(52.7077400330614,-6.41947076825076,11.0971961933879));
#26353=CARTESIAN_POINT('Ctrl Pts',(52.6180453654948,-6.35148029318637,11.));
#26354=CARTESIAN_POINT('Origin',(52.8690750612423,-6.60323306948161,14.5));
#26355=CARTESIAN_POINT('',(53.1320940795741,-6.26343186434448,24.2));
#26356=CARTESIAN_POINT('',(53.1320940795741,-6.26343186434448,14.5));
#26357=CARTESIAN_POINT('',(52.6060560429106,-6.94303427461875,24.2));
#26358=CARTESIAN_POINT('',(52.7010072733802,-6.82036427627618,24.2));
#26359=CARTESIAN_POINT('',(52.6060560429106,-6.94303427461875,11.5));
#26360=CARTESIAN_POINT('',(52.6060560429106,-6.94303427461874,14.5));
#26361=CARTESIAN_POINT('Ctrl Pts',(52.6060560429106,-6.94303427461875,11.5));
#26362=CARTESIAN_POINT('Ctrl Pts',(52.7299097311634,-6.78302442895846,11.4654707447276));
#26363=CARTESIAN_POINT('Ctrl Pts',(52.889681035389,-6.5766116681379,11.2969997378715));
#26364=CARTESIAN_POINT('Origin',(53.0783684845482,-7.45967821145953,11.25));
#26365=CARTESIAN_POINT('',(52.4819462572371,-7.82612128585083,11.5));
#26366=CARTESIAN_POINT('Origin',(53.0783684845482,-7.45967821145953,11.5));
#26367=CARTESIAN_POINT('',(52.6535843401555,-8.25652694495714,11.2969997378715));
#26368=CARTESIAN_POINT('Ctrl Pts',(52.6535843401555,-8.25652694495714,11.2969997378715));
#26369=CARTESIAN_POINT('Ctrl Pts',(52.5568973728928,-8.01407132459532,11.4654707447276));
#26370=CARTESIAN_POINT('Ctrl Pts',(52.4819462572371,-7.82612128585083,11.5));
#26371=CARTESIAN_POINT('Ctrl Pts',(52.6535843401555,-8.25652694495714,11.2969997378715));
#26372=CARTESIAN_POINT('Ctrl Pts',(52.5456731840226,-8.31036112214121,11.1987310576087));
#26373=CARTESIAN_POINT('Ctrl Pts',(52.4353775215618,-8.35743073608767,11.0971961933879));
#26374=CARTESIAN_POINT('Ctrl Pts',(52.3304167585326,-8.39806417445679,11.));
#26375=CARTESIAN_POINT('Origin',(53.0783684845482,-7.45967821145953,11.));
#26376=CARTESIAN_POINT('',(52.4819462572371,-7.82612128585083,24.2));
#26377=CARTESIAN_POINT('Origin',(53.0783684845482,-7.45967821145953,24.2));
#26378=CARTESIAN_POINT('',(52.4819462572371,-7.82612128585083,14.5));
#26379=CARTESIAN_POINT('Origin',(52.6411144591754,-8.22525703532526,14.5));
#26380=CARTESIAN_POINT('',(52.8002826611136,-8.6243927847997,24.2));
#26381=CARTESIAN_POINT('',(52.5394068040886,-7.97021136259661,24.2));
#26382=CARTESIAN_POINT('',(52.8002826611136,-8.6243927847997,11.5));
#26383=CARTESIAN_POINT('',(52.8002826611136,-8.6243927847997,14.5));
#26384=CARTESIAN_POINT('Ctrl Pts',(52.8002826611136,-8.6243927847997,11.5));
#26385=CARTESIAN_POINT('Ctrl Pts',(52.7267940781898,-8.44011024428003,11.3977655520829));
#26386=CARTESIAN_POINT('Ctrl Pts',(52.6535843401555,-8.25652694495714,11.2969997378715));
#26387=CARTESIAN_POINT('Origin',(52.2796703973459,-10.2751081719874,14.5));
#26388=CARTESIAN_POINT('',(52.302083191459,-10.2499890191339,11.2969997378715));
#26389=CARTESIAN_POINT('',(52.5657520484127,-9.95448198475414,11.5));
#26390=CARTESIAN_POINT('Ctrl Pts',(52.302083191459,-10.2499890191339,11.2969997378715));
#26391=CARTESIAN_POINT('Ctrl Pts',(52.4336670284067,-10.1025163525552,11.3977655520833));
#26392=CARTESIAN_POINT('Ctrl Pts',(52.5657520484127,-9.95448198475414,11.5));
#26393=CARTESIAN_POINT('',(52.5657520484127,-9.95448198475414,24.2));
#26394=CARTESIAN_POINT('',(52.5657520484127,-9.95448198475413,14.5));
#26395=CARTESIAN_POINT('',(51.9935887462792,-10.5957343592207,24.2));
#26396=CARTESIAN_POINT('',(52.0968657068422,-10.479986641844,24.2));
#26397=CARTESIAN_POINT('',(51.9935887462792,-10.5957343592207,11.5));
#26398=CARTESIAN_POINT('',(51.9935887462792,-10.5957343592207,14.5));
#26399=CARTESIAN_POINT('Ctrl Pts',(51.9935887462792,-10.5957343592207,11.5));
#26400=CARTESIAN_POINT('Ctrl Pts',(52.1283024557699,-10.4447538860551,11.4654707447276));
#26401=CARTESIAN_POINT('Ctrl Pts',(52.302083191459,-10.2499890191339,11.2969997378715));
#26402=CARTESIAN_POINT('Origin',(52.428711399332,-11.1440666278319,11.25));
#26403=CARTESIAN_POINT('',(51.8081802498931,-11.4680127538716,11.5));
#26404=CARTESIAN_POINT('Origin',(52.428711399332,-11.1440666278319,11.5));
#26405=CARTESIAN_POINT('',(51.9493766500092,-11.909342833849,11.2969997378715));
#26406=CARTESIAN_POINT('Ctrl Pts',(51.9493766500092,-11.909342833849,11.2969997378715));
#26407=CARTESIAN_POINT('Ctrl Pts',(51.8698380564552,-11.6607332812994,11.4654707447276));
#26408=CARTESIAN_POINT('Ctrl Pts',(51.8081802498931,-11.4680127538716,11.5));
#26409=CARTESIAN_POINT('Ctrl Pts',(51.9493766500092,-11.909342833849,11.2969997378715));
#26410=CARTESIAN_POINT('Ctrl Pts',(51.8379730776617,-11.9555183719537,11.1987310576086));
#26411=CARTESIAN_POINT('Ctrl Pts',(51.7246626796018,-11.9947794902037,11.0971961933879));
#26412=CARTESIAN_POINT('Ctrl Pts',(51.6171231503394,-12.0279922548488,11.));
#26413=CARTESIAN_POINT('Ctrl Pts',(52.3020831914591,-10.2499890191339,11.2969997378715));
#26414=CARTESIAN_POINT('Ctrl Pts',(52.2190922473368,-10.162493651001,11.1987310576086));
#26415=CARTESIAN_POINT('Ctrl Pts',(52.1315469833259,-10.0805393438292,11.0971961933879));
#26416=CARTESIAN_POINT('Ctrl Pts',(52.0468135832502,-10.0064577064218,11.));
#26417=CARTESIAN_POINT('Origin',(52.428711399332,-11.1440666278319,11.));
#26418=CARTESIAN_POINT('',(51.8081802498931,-11.4680127538716,24.2));
#26419=CARTESIAN_POINT('Origin',(52.428711399332,-11.1440666278319,24.2));
#26420=CARTESIAN_POINT('',(51.8081802498931,-11.4680127538716,14.5));
#26421=CARTESIAN_POINT('Origin',(51.9391184236626,-11.8772792412203,14.5));
#26422=CARTESIAN_POINT('',(52.0700565974321,-12.2865457285691,24.2));
#26423=CARTESIAN_POINT('',(51.8554496100851,-11.6157600795601,24.2));
#26424=CARTESIAN_POINT('',(52.0700565974321,-12.2865457285691,11.5));
#26425=CARTESIAN_POINT('',(52.0700565974321,-12.2865457285691,14.5));
#26426=CARTESIAN_POINT('Ctrl Pts',(52.0700565974321,-12.2865457285691,11.5));
#26427=CARTESIAN_POINT('Ctrl Pts',(52.0096019292023,-12.0975857866519,11.3977655520834));
#26428=CARTESIAN_POINT('Ctrl Pts',(51.9493766500092,-11.909342833849,11.2969997378715));
#26429=CARTESIAN_POINT('Origin',(51.4355644344077,-13.8969239803298,14.5));
#26430=CARTESIAN_POINT('',(51.4596748556075,-13.8734294539541,11.2969997378716));
#26431=CARTESIAN_POINT('',(51.7433149571623,-13.5970348695555,11.5));
#26432=CARTESIAN_POINT('Ctrl Pts',(51.4596748556075,-13.8734294539541,11.2969997378716));
#26433=CARTESIAN_POINT('Ctrl Pts',(51.6012253341357,-13.7354948478467,11.3977655520833));
#26434=CARTESIAN_POINT('Ctrl Pts',(51.7433149571623,-13.5970348695555,11.5));
#26435=CARTESIAN_POINT('',(51.7433149571623,-13.5970348695555,24.2));
#26436=CARTESIAN_POINT('',(51.7433149571622,-13.5970348695555,14.5));
#26437=CARTESIAN_POINT('',(51.1278139116531,-14.1968130911041,24.2));
#26438=CARTESIAN_POINT('',(51.238913447339,-14.0885515659373,24.2));
#26439=CARTESIAN_POINT('',(51.1278139116531,-14.1968130911041,11.5));
#26440=CARTESIAN_POINT('',(51.1278139116531,-14.1968130911041,14.5));
#26441=CARTESIAN_POINT('Ctrl Pts',(51.1278139116531,-14.1968130911041,11.5));
#26442=CARTESIAN_POINT('Ctrl Pts',(51.2727313307305,-14.055597552122,11.4654707447276));
#26443=CARTESIAN_POINT('Ctrl Pts',(51.4596748556075,-13.8734294539541,11.2969997378716));
#26444=CARTESIAN_POINT('Origin',(51.5236269022939,-14.7741622717911,11.25));
#26445=CARTESIAN_POINT('',(50.8820099961117,-15.054033216516,11.5));
#26446=CARTESIAN_POINT('Origin',(51.5236269022939,-14.7741622717911,11.5));
#26447=CARTESIAN_POINT('',(50.9920768187571,-15.5041376015772,11.2969997378715));
#26448=CARTESIAN_POINT('Ctrl Pts',(50.9920768187571,-15.5041376015772,11.2969997378715));
#26449=CARTESIAN_POINT('Ctrl Pts',(50.9300741029444,-15.2505853175897,11.4654707447276));
#26450=CARTESIAN_POINT('Ctrl Pts',(50.8820099961117,-15.054033216516,11.5));
#26451=CARTESIAN_POINT('Ctrl Pts',(50.9920768187571,-15.5041376015772,11.2969997378715));
#26452=CARTESIAN_POINT('Ctrl Pts',(50.8777235772014,-15.5424295380224,11.1987310576086));
#26453=CARTESIAN_POINT('Ctrl Pts',(50.7619504804118,-15.5736908843544,11.0971961933879));
#26454=CARTESIAN_POINT('Ctrl Pts',(50.6523561066928,-15.5993211660246,11.));
#26455=CARTESIAN_POINT('Ctrl Pts',(51.4596748556075,-13.8734294539541,11.2969997378716));
#26456=CARTESIAN_POINT('Ctrl Pts',(51.3829894416039,-13.7803580645257,11.1987310576087));
#26457=CARTESIAN_POINT('Ctrl Pts',(51.3013742769325,-13.6924965450168,11.097196193388));
#26458=CARTESIAN_POINT('Ctrl Pts',(51.2220149569554,-13.6126846635571,11.));
#26459=CARTESIAN_POINT('Origin',(51.5236269022939,-14.7741622717911,11.));
#26460=CARTESIAN_POINT('',(50.8820099961117,-15.054033216516,24.2));
#26461=CARTESIAN_POINT('Origin',(51.5236269022939,-14.7741622717911,24.2));
#26462=CARTESIAN_POINT('',(50.8820099961117,-15.054033216516,14.5));
#26463=CARTESIAN_POINT('Origin',(50.9840802240917,-15.4714365365519,14.5));
#26464=CARTESIAN_POINT('',(51.0861504520717,-15.8888398565878,24.2));
#26465=CARTESIAN_POINT('',(50.9188578780728,-15.204717981028,24.2));
#26466=CARTESIAN_POINT('',(51.0861504520717,-15.8888398565878,11.5));
#26467=CARTESIAN_POINT('',(51.0861504520717,-15.8888398565878,14.5));
#26468=CARTESIAN_POINT('Ctrl Pts',(51.0861504520717,-15.8888398565878,11.5));
#26469=CARTESIAN_POINT('Ctrl Pts',(51.039024227602,-15.6961231071132,11.3977655520826));
#26470=CARTESIAN_POINT('Ctrl Pts',(50.9920768187571,-15.5041376015772,11.2969997378715));
#26471=CARTESIAN_POINT('Origin',(50.34086957183,-17.4510353719535,14.5));
#26472=CARTESIAN_POINT('',(50.3665601565676,-17.4292799350267,11.2969997378715));
#26473=CARTESIAN_POINT('',(50.6687896366606,-17.1733443672407,11.5));
#26474=CARTESIAN_POINT('Ctrl Pts',(50.3665601565676,-17.4292799350267,11.2969997378715));
#26475=CARTESIAN_POINT('Ctrl Pts',(50.5173876569724,-17.3015553929273,11.3977655520822));
#26476=CARTESIAN_POINT('Ctrl Pts',(50.6687896366606,-17.1733443672407,11.5));
#26477=CARTESIAN_POINT('',(50.6687896366606,-17.1733443672407,24.2));
#26478=CARTESIAN_POINT('',(50.6687896366606,-17.1733443672407,14.5));
#26479=CARTESIAN_POINT('',(50.0129495069995,-17.7287263766662,24.2));
#26480=CARTESIAN_POINT('',(50.131330352038,-17.6284784829776,24.2));
#26481=CARTESIAN_POINT('',(50.0129495069995,-17.7287263766662,11.5));
#26482=CARTESIAN_POINT('',(50.0129495069995,-17.7287263766662,14.5));
#26483=CARTESIAN_POINT('Ctrl Pts',(50.0129495069995,-17.7287263766662,11.5));
#26484=CARTESIAN_POINT('Ctrl Pts',(50.1673646125647,-17.5979637597785,11.4654707447276));
#26485=CARTESIAN_POINT('Ctrl Pts',(50.3665601565676,-17.4292799350267,11.2969997378715));
#26486=CARTESIAN_POINT('Origin',(50.3675244741247,-18.3322796822558,11.25));
#26487=CARTESIAN_POINT('',(49.7079477042709,-18.5667119425557,11.5));
#26488=CARTESIAN_POINT('Origin',(50.3675244741247,-18.3322796822558,11.5));
#26489=CARTESIAN_POINT('',(49.7863487149498,-19.023397769381,11.2969997378715));
#26490=CARTESIAN_POINT('Ctrl Pts',(49.7863487149498,-19.023397769381,11.2969997378715));
#26491=CARTESIAN_POINT('Ctrl Pts',(49.7421839478773,-18.7661380351961,11.4654707447276));
#26492=CARTESIAN_POINT('Ctrl Pts',(49.7079477042709,-18.5667119425557,11.5));
#26493=CARTESIAN_POINT('Ctrl Pts',(49.7863487149498,-19.023397769381,11.2969997378715));
#26494=CARTESIAN_POINT('Ctrl Pts',(49.6696029216838,-19.0536195497014,11.1987310576087));
#26495=CARTESIAN_POINT('Ctrl Pts',(49.5519311610547,-19.0767288219785,11.0971961933879));
#26496=CARTESIAN_POINT('Ctrl Pts',(49.4408158756514,-19.0946517525179,11.));
#26497=CARTESIAN_POINT('Ctrl Pts',(50.3665601565676,-17.4292799350267,11.2969997378715));
#26498=CARTESIAN_POINT('Ctrl Pts',(50.2965538763113,-17.3310859587567,11.1987310576086));
#26499=CARTESIAN_POINT('Ctrl Pts',(50.2212664318579,-17.2377452794019,11.0971961933879));
#26500=CARTESIAN_POINT('Ctrl Pts',(50.1476678226092,-17.1525919893539,11.));
#26501=CARTESIAN_POINT('Origin',(50.3675244741247,-18.3322796822558,11.));
#26502=CARTESIAN_POINT('',(49.7079477042709,-18.5667119425557,24.2));
#26503=CARTESIAN_POINT('Origin',(50.3675244741247,-18.3322796822558,24.2));
#26504=CARTESIAN_POINT('',(49.7079477042709,-18.5667119425557,14.5));
#26505=CARTESIAN_POINT('Origin',(49.7806527105709,-18.9902185482606,14.5));
#26506=CARTESIAN_POINT('',(49.8533577168708,-19.4137251539655,24.2));
#26507=CARTESIAN_POINT('',(49.7341945888243,-18.7196000248653,24.2));
#26508=CARTESIAN_POINT('',(49.8533577168708,-19.4137251539655,11.5));
#26509=CARTESIAN_POINT('',(49.8533577168709,-19.4137251539655,14.5));
#26510=CARTESIAN_POINT('Ctrl Pts',(49.8533577168708,-19.4137251539655,11.5));
#26511=CARTESIAN_POINT('Ctrl Pts',(49.8197895303902,-19.2181904935674,11.3977655520828));
#26512=CARTESIAN_POINT('Ctrl Pts',(49.7863487149498,-19.023397769381,11.2969997378715));
#26513=CARTESIAN_POINT('Origin',(49.0009190529448,-20.9201270734171,14.5));
#26514=CARTESIAN_POINT('',(49.028064639274,-20.900216716241,11.2969997378715));
#26515=CARTESIAN_POINT('',(49.3474110662579,-20.6659870574277,11.5));
#26516=CARTESIAN_POINT('Ctrl Pts',(49.028064639274,-20.900216716241,11.2969997378715));
#26517=CARTESIAN_POINT('Ctrl Pts',(49.1874343451367,-20.7833244992779,11.3977655520828));
#26518=CARTESIAN_POINT('Ctrl Pts',(49.3474110662579,-20.6659870574277,11.5));
#26519=CARTESIAN_POINT('',(49.3474110662579,-20.6659870574277,24.2));
#26520=CARTESIAN_POINT('',(49.3474110662579,-20.6659870574277,14.5));
#26521=CARTESIAN_POINT('',(48.6544270396318,-21.1742670894066,24.2));
#26522=CARTESIAN_POINT('',(48.7795124544456,-21.0825212248573,24.2));
#26523=CARTESIAN_POINT('',(48.6544270396318,-21.1742670894066,11.5));
#26524=CARTESIAN_POINT('',(48.6544270396318,-21.1742670894066,14.5));
#26525=CARTESIAN_POINT('Ctrl Pts',(48.6544270396318,-21.1742670894066,11.5));
#26526=CARTESIAN_POINT('Ctrl Pts',(48.8175875368124,-21.0545944569386,11.4654707447276));
#26527=CARTESIAN_POINT('Ctrl Pts',(49.028064639274,-20.900216716241,11.2969997378715));
#26528=CARTESIAN_POINT('Origin',(48.9660365296434,-21.8010840688629,11.25));
#26529=CARTESIAN_POINT('',(48.2917132878404,-21.9889355143306,11.5));
#26530=CARTESIAN_POINT('Origin',(48.9660365296434,-21.8010840688629,11.5));
#26531=CARTESIAN_POINT('',(48.3380665247095,-22.4499778554777,11.2969997378716));
#26532=CARTESIAN_POINT('Ctrl Pts',(48.3380665247095,-22.4499778554777,11.2969997378716));
#26533=CARTESIAN_POINT('Ctrl Pts',(48.3119548726829,-22.1902640146607,11.4654707447277));
#26534=CARTESIAN_POINT('Ctrl Pts',(48.2917132878404,-21.9889355143306,11.5));
#26535=CARTESIAN_POINT('Ctrl Pts',(48.3380665247095,-22.4499778554777,11.2969997378716));
#26536=CARTESIAN_POINT('Ctrl Pts',(48.2194969535028,-22.4719822421975,11.1987310576087));
#26537=CARTESIAN_POINT('Ctrl Pts',(48.1004998140236,-22.486826854368,11.0971961933879));
#26538=CARTESIAN_POINT('Ctrl Pts',(47.9884049594373,-22.4969551150606,11.));
#26539=CARTESIAN_POINT('Ctrl Pts',(49.028064639274,-20.900216716241,11.2969997378714));
#26540=CARTESIAN_POINT('Ctrl Pts',(48.9650785563254,-20.7973785443114,11.1987310576086));
#26541=CARTESIAN_POINT('Ctrl Pts',(48.8964856249515,-20.699013451518,11.0971961933879));
#26542=CARTESIAN_POINT('Ctrl Pts',(48.8290062914572,-20.608933611151,11.));
#26543=CARTESIAN_POINT('Origin',(48.9660365296434,-21.8010840688629,11.));
#26544=CARTESIAN_POINT('',(48.2917132878404,-21.9889355143306,24.2));
#26545=CARTESIAN_POINT('Origin',(48.9660365296434,-21.8010840688629,24.2));
#26546=CARTESIAN_POINT('',(48.2917132878404,-21.9889355143306,14.5));
#26547=CARTESIAN_POINT('Origin',(47.4222409819888,-24.287298018663,14.5));
#26548=CARTESIAN_POINT('',(47.0588650944528,-24.5166489013173,11.0622545443403));
#26549=CARTESIAN_POINT('',(47.7856168695248,-24.0579471360087,11.5));
#26550=CARTESIAN_POINT('Ctrl Pts',(47.0588650944528,-24.5166489013173,11.0622545443403));
#26551=CARTESIAN_POINT('Ctrl Pts',(47.4207482757382,-24.2882401656459,11.2776618075213));
#26552=CARTESIAN_POINT('Ctrl Pts',(47.7856168695248,-24.0579471360087,11.5));
#26553=CARTESIAN_POINT('',(47.7856168695248,-24.0579471360087,24.2));
#26554=CARTESIAN_POINT('',(47.7856168695248,-24.0579471360087,14.5));
#26555=CARTESIAN_POINT('',(47.0588650944529,-24.5166489013173,24.2));
#26556=CARTESIAN_POINT('',(47.1900456754746,-24.4338520425371,24.2));
#26557=CARTESIAN_POINT('',(47.0588650944529,-24.5166489013173,14.5));
#26558=CARTESIAN_POINT('Origin',(0.,0.,14.5));
#26559=CARTESIAN_POINT('',(48.3776844341154,-22.8440287338541,11.5));
#26560=CARTESIAN_POINT('Origin',(0.,0.,11.5));
#26561=CARTESIAN_POINT('',(48.3776844341154,-22.8440287338541,24.2));
#26562=CARTESIAN_POINT('',(48.3776844341154,-22.8440287338541,14.5));
#26563=CARTESIAN_POINT('Origin',(0.,0.,24.2));
#26564=CARTESIAN_POINT('Origin',(0.,0.,11.25));
#26565=CARTESIAN_POINT('Ctrl Pts',(46.9634710240919,-24.5648608660681,11.));
#26566=CARTESIAN_POINT('Ctrl Pts',(46.9953053071723,-24.5455885286143,11.0192759649605));
#26567=CARTESIAN_POINT('Ctrl Pts',(47.0275356235898,-24.5295833141324,11.0404458048696));
#26568=CARTESIAN_POINT('Ctrl Pts',(47.0588650944527,-24.5166489013174,11.0622545443404));
#26569=CARTESIAN_POINT('Ctrl Pts',(48.3776844341154,-22.8440287338541,11.5));
#26570=CARTESIAN_POINT('Ctrl Pts',(48.3578378264539,-22.6466287877422,11.3977655520828));
#26571=CARTESIAN_POINT('Ctrl Pts',(48.3380665247095,-22.4499778554777,11.2969997378716));
#26572=CARTESIAN_POINT('Origin',(48.3346988609779,-22.4164821240923,14.5));
#26573=CARTESIAN_POINT('',(48.3072313028028,-22.1432820590691,24.2));
#26574=CARTESIAN_POINT('Origin',(52.2796703973459,10.2751081719876,14.5));
#26575=CARTESIAN_POINT('',(52.5657520484127,9.95448198475442,24.2));
#26576=CARTESIAN_POINT('',(51.9935887462791,10.5957343592208,24.2));
#26577=CARTESIAN_POINT('',(52.0968657068422,10.479986641844,24.2));
#26578=CARTESIAN_POINT('',(52.5657520484127,9.95448198475442,11.5));
#26579=CARTESIAN_POINT('',(52.5657520484127,9.95448198475442,14.5));
#26580=CARTESIAN_POINT('',(51.993588746279,10.5957343592209,11.0622545443402));
#26581=CARTESIAN_POINT('Ctrl Pts',(52.5657520484127,9.95448198475442,11.5));
#26582=CARTESIAN_POINT('Ctrl Pts',(52.278495206905,10.2764252674005,11.2776618075198));
#26583=CARTESIAN_POINT('Ctrl Pts',(51.993588746279,10.5957343592209,11.0622545443402));
#26584=CARTESIAN_POINT('',(51.9935887462791,10.5957343592208,14.5));
#26585=CARTESIAN_POINT('Origin',(0.,0.,11.25));
#26586=CARTESIAN_POINT('',(52.8002826611136,8.62439278479999,11.5));
#26587=CARTESIAN_POINT('Origin',(0.,0.,11.5));
#26588=CARTESIAN_POINT('',(52.6535843401555,8.25652694495716,11.2969997378715));
#26589=CARTESIAN_POINT('Ctrl Pts',(52.6535843401555,8.25652694495716,11.2969997378715));
#26590=CARTESIAN_POINT('Ctrl Pts',(52.7267940781897,8.4401102442802,11.3977655520829));
#26591=CARTESIAN_POINT('Ctrl Pts',(52.8002826611136,8.62439278479999,11.5));
#26592=CARTESIAN_POINT('Ctrl Pts',(52.6535843401555,8.25652694495715,11.2969997378715));
#26593=CARTESIAN_POINT('Ctrl Pts',(52.5456731840225,8.31036112214122,11.1987310576086));
#26594=CARTESIAN_POINT('Ctrl Pts',(52.4353775215617,8.35743073608767,11.0971961933879));
#26595=CARTESIAN_POINT('Ctrl Pts',(52.3304167585326,8.39806417445676,11.));
#26596=CARTESIAN_POINT('Ctrl Pts',(51.993588746279,10.5957343592209,11.0622545443403));
#26597=CARTESIAN_POINT('Ctrl Pts',(51.9670381333318,10.6168032873272,11.0404458048695));
#26598=CARTESIAN_POINT('Ctrl Pts',(51.9404679997109,10.6410723661384,11.0192759649605));
#26599=CARTESIAN_POINT('Ctrl Pts',(51.9151790989041,10.6683728435365,11.));
#26600=CARTESIAN_POINT('Origin',(0.,0.,14.5));
#26601=CARTESIAN_POINT('',(52.8002826611136,8.62439278479999,24.2));
#26602=CARTESIAN_POINT('Origin',(0.,0.,24.2));
#26603=CARTESIAN_POINT('',(52.8002826611136,8.62439278479999,14.5));
#26604=CARTESIAN_POINT('Origin',(52.6411144591754,8.22525703532543,14.5));
#26605=CARTESIAN_POINT('',(52.4819462572372,7.82612128585089,24.2));
#26606=CARTESIAN_POINT('',(52.5394068040886,7.97021136259661,24.2));
#26607=CARTESIAN_POINT('',(52.4819462572372,7.82612128585089,11.5));
#26608=CARTESIAN_POINT('',(52.4819462572372,7.82612128585088,14.5));
#26609=CARTESIAN_POINT('Ctrl Pts',(52.4819462572372,7.82612128585089,11.5));
#26610=CARTESIAN_POINT('Ctrl Pts',(52.5568973728928,8.01407132459532,11.4654707447276));
#26611=CARTESIAN_POINT('Ctrl Pts',(52.6535843401555,8.25652694495716,11.2969997378715));
#26612=CARTESIAN_POINT('Origin',(52.8690750612423,6.60323306948177,14.5));
#26613=CARTESIAN_POINT('',(53.1320940795741,6.26343186434477,24.2));
#26614=CARTESIAN_POINT('',(52.6060560429105,6.94303427461878,24.2));
#26615=CARTESIAN_POINT('',(52.7010072733802,6.82036427627619,24.2));
#26616=CARTESIAN_POINT('',(53.1320940795741,6.26343186434477,11.5));
#26617=CARTESIAN_POINT('',(53.1320940795741,6.26343186434477,14.5));
#26618=CARTESIAN_POINT('',(52.889681035389,6.57661166813793,11.2969997378715));
#26619=CARTESIAN_POINT('Ctrl Pts',(53.1320940795741,6.26343186434477,11.5));
#26620=CARTESIAN_POINT('Ctrl Pts',(53.0106571675283,6.42031941309698,11.3977655520827));
#26621=CARTESIAN_POINT('Ctrl Pts',(52.889681035389,6.57661166813793,11.2969997378715));
#26622=CARTESIAN_POINT('',(52.6060560429105,6.94303427461878,11.5));
#26623=CARTESIAN_POINT('Ctrl Pts',(52.889681035389,6.57661166813793,11.2969997378715));
#26624=CARTESIAN_POINT('Ctrl Pts',(52.7299097311634,6.78302442895845,11.4654707447276));
#26625=CARTESIAN_POINT('Ctrl Pts',(52.6060560429105,6.94303427461878,11.5));
#26626=CARTESIAN_POINT('',(52.6060560429105,6.94303427461878,14.5));
#26627=CARTESIAN_POINT('Origin',(0.,0.,11.25));
#26628=CARTESIAN_POINT('',(53.273271055136,4.920222666304,11.5));
#26629=CARTESIAN_POINT('Origin',(0.,0.,11.5));
#26630=CARTESIAN_POINT('',(53.1012690601164,4.56348608673264,11.2969997378715));
#26631=CARTESIAN_POINT('Ctrl Pts',(53.1012690601164,4.56348608673264,11.2969997378715));
#26632=CARTESIAN_POINT('Ctrl Pts',(53.1871065865071,4.74151533319583,11.3977655520826));
#26633=CARTESIAN_POINT('Ctrl Pts',(53.273271055136,4.920222666304,11.5));
#26634=CARTESIAN_POINT('Ctrl Pts',(53.1012690601164,4.56348608673263,11.2969997378715));
#26635=CARTESIAN_POINT('Ctrl Pts',(52.9973760525035,4.62471662829628,11.1987310576087));
#26636=CARTESIAN_POINT('Ctrl Pts',(52.8906324750223,4.67936541951142,11.0971961933879));
#26637=CARTESIAN_POINT('Ctrl Pts',(52.7887618365133,4.72722156957729,11.));
#26638=CARTESIAN_POINT('Ctrl Pts',(52.889681035389,6.57661166813793,11.2969997378715));
#26639=CARTESIAN_POINT('Ctrl Pts',(52.8007888846856,6.49511858993887,11.1987310576087));
#26640=CARTESIAN_POINT('Ctrl Pts',(52.7077400330614,6.41947076825075,11.0971961933879));
#26641=CARTESIAN_POINT('Ctrl Pts',(52.6180453654948,6.35148029318636,11.));
#26642=CARTESIAN_POINT('Origin',(0.,0.,14.5));
#26643=CARTESIAN_POINT('',(53.273271055136,4.920222666304,24.2));
#26644=CARTESIAN_POINT('Origin',(0.,0.,24.2));
#26645=CARTESIAN_POINT('',(53.273271055136,4.920222666304,14.5));
#26646=CARTESIAN_POINT('Origin',(53.0866482765093,4.5331622039542,14.5));
#26647=CARTESIAN_POINT('',(52.9000254978827,4.1461017416044,24.2));
#26648=CARTESIAN_POINT('',(52.9673972893853,4.2858325770374,24.2));
#26649=CARTESIAN_POINT('',(52.9000254978827,4.1461017416044,11.5));
#26650=CARTESIAN_POINT('',(52.9000254978827,4.1461017416044,14.5));
#26651=CARTESIAN_POINT('Ctrl Pts',(52.9000254978827,4.1461017416044,11.5));
#26652=CARTESIAN_POINT('Ctrl Pts',(52.9879047683306,4.32836561796949,11.4654707447276));
#26653=CARTESIAN_POINT('Ctrl Pts',(53.1012690601164,4.56348608673264,11.2969997378715));
#26654=CARTESIAN_POINT('Origin',(53.2009069058212,2.89918767921592,14.5));
#26655=CARTESIAN_POINT('',(53.4395818891992,2.54186693348969,24.2));
#26656=CARTESIAN_POINT('',(52.9622319224432,3.25650842494215,24.2));
#26657=CARTESIAN_POINT('',(53.048394829969,3.12751378153496,24.2));
#26658=CARTESIAN_POINT('',(53.4395818891992,2.54186693348969,11.5));
#26659=CARTESIAN_POINT('',(53.4395818891992,2.54186693348969,14.5));
#26660=CARTESIAN_POINT('',(53.2196056697666,2.87119372617337,11.2969997378715));
#26661=CARTESIAN_POINT('Ctrl Pts',(53.4395818891992,2.54186693348969,11.5));
#26662=CARTESIAN_POINT('Ctrl Pts',(53.3293847135434,2.70684332282464,11.3977655520829));
#26663=CARTESIAN_POINT('Ctrl Pts',(53.2196056697666,2.87119372617337,11.2969997378715));
#26664=CARTESIAN_POINT('',(52.9622319224432,3.25650842494215,11.5));
#26665=CARTESIAN_POINT('Ctrl Pts',(53.2196056697666,2.87119372617337,11.2969997378715));
#26666=CARTESIAN_POINT('Ctrl Pts',(53.0746221867387,3.08824875867107,11.4654707447276));
#26667=CARTESIAN_POINT('Ctrl Pts',(52.9622319224432,3.25650842494215,11.5));
#26668=CARTESIAN_POINT('',(52.9622319224432,3.25650842494215,14.5));
#26669=CARTESIAN_POINT('Origin',(0.,0.,11.25));
#26670=CARTESIAN_POINT('',(53.4867174275882,1.19208171755715,11.5));
#26671=CARTESIAN_POINT('Origin',(0.,0.,11.5));
#26672=CARTESIAN_POINT('',(53.0603811317944,0.445882806437465,11.0622545443402));
#26673=CARTESIAN_POINT('Ctrl Pts',(53.0603811317944,0.445882806437465,11.0622545443402));
#26674=CARTESIAN_POINT('Ctrl Pts',(53.2726736095176,0.817449612451526,11.277661807522));
#26675=CARTESIAN_POINT('Ctrl Pts',(53.4867174275882,1.19208171755715,11.5));
#26676=CARTESIAN_POINT('Ctrl Pts',(52.9987873134328,0.358529364921033,11.));
#26677=CARTESIAN_POINT('Ctrl Pts',(53.0178475026662,0.390491119512532,11.0192759649605));
#26678=CARTESIAN_POINT('Ctrl Pts',(53.0387911899085,0.419754102130115,11.0404458048696));
#26679=CARTESIAN_POINT('Ctrl Pts',(53.0603811317944,0.445882806437441,11.0622545443403));
#26680=CARTESIAN_POINT('Ctrl Pts',(52.9329273198661,2.66555910641111,11.));
#26681=CARTESIAN_POINT('Ctrl Pts',(53.0271462715192,2.7271271763723,11.0971961933878));
#26682=CARTESIAN_POINT('Ctrl Pts',(53.1252453861049,2.79609996399359,11.1987310576086));
#26683=CARTESIAN_POINT('Ctrl Pts',(53.2196056697666,2.87119372617338,11.2969997378715));
#26684=CARTESIAN_POINT('Origin',(0.,0.,14.5));
#26685=CARTESIAN_POINT('',(53.4867174275882,1.19208171755715,24.2));
#26686=CARTESIAN_POINT('Origin',(0.,0.,24.2));
#26687=CARTESIAN_POINT('',(53.4867174275882,1.19208171755715,14.5));
#26688=CARTESIAN_POINT('Origin',(53.2735492796914,-0.818982261997365,14.5));
#26689=CARTESIAN_POINT('',(53.0603811317945,-0.44588280643758,11.0622545443404));
#26690=CARTESIAN_POINT('',(53.0603811317945,-0.44588280643758,24.2));
#26691=CARTESIAN_POINT('',(53.0603811317945,-0.44588280643758,14.5));
#26692=CARTESIAN_POINT('',(53.4867174275882,-1.19208171755715,24.2));
#26693=CARTESIAN_POINT('',(53.1373359393522,-0.580573645973269,24.2));
#26694=CARTESIAN_POINT('',(53.4867174275882,-1.19208171755715,11.5));
#26695=CARTESIAN_POINT('',(53.4867174275882,-1.19208171755715,14.5));
#26696=CARTESIAN_POINT('Ctrl Pts',(53.4867174275882,-1.19208171755715,11.5));
#26697=CARTESIAN_POINT('Ctrl Pts',(53.3449516913153,-0.943954970938041,
11.3527407245752));
#26698=CARTESIAN_POINT('Ctrl Pts',(53.2028335182235,-0.695211368627667,
11.2067970124649));
#26699=CARTESIAN_POINT('Ctrl Pts',(53.0603811317945,-0.44588280643758,11.0622545443404));
#26700=CARTESIAN_POINT('Origin',(0.,0.,11.25));
#26701=CARTESIAN_POINT('Ctrl Pts',(52.9987873134328,-0.358529364921033,
11.));
#26702=CARTESIAN_POINT('Ctrl Pts',(53.0178472961609,-0.390490773226817,
11.0192757561174));
#26703=CARTESIAN_POINT('Ctrl Pts',(53.0387914082603,-0.419754366385171,
11.0404460254342));
#26704=CARTESIAN_POINT('Ctrl Pts',(53.0603811317945,-0.44588280643758,11.0622545443404));
#26705=CARTESIAN_POINT('Origin',(0.,0.,11.5));
#26706=CARTESIAN_POINT('Origin',(0.,0.,11.25));
#26707=CARTESIAN_POINT('Origin',(0.,0.,11.5));
#26708=CARTESIAN_POINT('Origin',(0.,0.,11.25));
#26709=CARTESIAN_POINT('Origin',(0.,0.,11.5));
#26710=CARTESIAN_POINT('Origin',(0.,0.,11.25));
#26711=CARTESIAN_POINT('Origin',(0.,0.,11.5));
#26712=CARTESIAN_POINT('Origin',(0.,0.,11.25));
#26713=CARTESIAN_POINT('Origin',(0.,0.,11.5));
#26714=CARTESIAN_POINT('Origin',(0.,0.,14.5));
#26715=CARTESIAN_POINT('Origin',(0.,0.,24.2));
#26716=CARTESIAN_POINT('Origin',(0.,0.,14.5));
#26717=CARTESIAN_POINT('Origin',(0.,0.,24.2));
#26718=CARTESIAN_POINT('Origin',(0.,0.,14.5));
#26719=CARTESIAN_POINT('Origin',(0.,0.,24.2));
#26720=CARTESIAN_POINT('Origin',(0.,0.,14.5));
#26721=CARTESIAN_POINT('Origin',(0.,0.,24.2));
#26722=CARTESIAN_POINT('Origin',(0.,0.,14.5));
#26723=CARTESIAN_POINT('Origin',(0.,0.,24.2));
#26724=CARTESIAN_POINT('Origin',(0.,0.,14.5));
#26725=CARTESIAN_POINT('Origin',(0.,0.,24.2));
#26726=CARTESIAN_POINT('Origin',(53.2735492796914,0.818982261997365,14.5));
#26727=CARTESIAN_POINT('',(53.0603811317945,0.44588280643758,24.2));
#26728=CARTESIAN_POINT('',(53.1373359393522,0.580573645973269,24.2));
#26729=CARTESIAN_POINT('',(53.0603811317945,0.44588280643758,14.5));
#26730=CARTESIAN_POINT('Origin',(53.0783684845482,7.45967821145951,11.25));
#26731=CARTESIAN_POINT('Origin',(53.0783684845482,7.45967821145951,11.5));
#26732=CARTESIAN_POINT('Origin',(53.4694330939266,3.73894699268512,11.25));
#26733=CARTESIAN_POINT('Origin',(53.4694330939266,3.73894699268512,11.5));
#26734=CARTESIAN_POINT('Origin',(53.6,0.,11.));
#26735=CARTESIAN_POINT('Origin',(53.6,0.,24.2));
#26736=CARTESIAN_POINT('Origin',(53.4694330939266,3.73894699268512,11.));
#26737=CARTESIAN_POINT('Origin',(53.4694330939266,3.73894699268512,24.2));
#26738=CARTESIAN_POINT('Origin',(53.0783684845482,7.45967821145951,11.));
#26739=CARTESIAN_POINT('Origin',(53.0783684845482,7.45967821145951,24.2));
#26740=CARTESIAN_POINT('Origin',(40.2834747403675,34.8709542118271,14.5));
#26741=CARTESIAN_POINT('',(40.2774792716873,34.9040806293113,11.2969997378715));
#26742=CARTESIAN_POINT('',(40.2069473082991,35.2937868207374,11.5));
#26743=CARTESIAN_POINT('Ctrl Pts',(40.2774792716873,34.9040806293113,11.2969997378715));
#26744=CARTESIAN_POINT('Ctrl Pts',(40.2422803237447,35.0985633473016,11.3977655520825));
#26745=CARTESIAN_POINT('Ctrl Pts',(40.2069473082991,35.2937868207374,11.5));
#26746=CARTESIAN_POINT('',(40.2069473082991,35.2937868207374,24.2));
#26747=CARTESIAN_POINT('',(40.2069473082991,35.2937868207374,14.5));
#26748=CARTESIAN_POINT('',(40.3600021724359,34.4481216029168,24.2));
#26749=CARTESIAN_POINT('',(40.332375372345,34.600766368886,24.2));
#26750=CARTESIAN_POINT('',(40.3600021724359,34.4481216029168,11.5));
#26751=CARTESIAN_POINT('',(40.3600021724359,34.4481216029168,14.5));
#26752=CARTESIAN_POINT('Ctrl Pts',(40.3600021724359,34.4481216029168,11.5));
#26753=CARTESIAN_POINT('Ctrl Pts',(40.3239659771285,34.6472303155083,11.4654707447276));
#26754=CARTESIAN_POINT('Ctrl Pts',(40.2774792716873,34.9040806293113,11.2969997378715));
#26755=CARTESIAN_POINT('Origin',(41.0599821511772,34.4534158791985,11.25));
#26756=CARTESIAN_POINT('',(40.9332180591367,33.7649895106091,11.5));
#26757=CARTESIAN_POINT('Origin',(41.0599821511772,34.4534158791985,11.5));
#26758=CARTESIAN_POINT('',(41.3679200920551,33.6045438641267,11.2969997378715));
#26759=CARTESIAN_POINT('Ctrl Pts',(41.3679200920551,33.6045438641267,11.2969997378715));
#26760=CARTESIAN_POINT('Ctrl Pts',(41.1230442433439,33.6949259209821,11.4654707447276));
#26761=CARTESIAN_POINT('Ctrl Pts',(40.9332180591367,33.7649895106091,11.5));
#26762=CARTESIAN_POINT('Ctrl Pts',(41.3679200920551,33.6045438641267,11.2969997378715));
#26763=CARTESIAN_POINT('Ctrl Pts',(41.3357200249272,33.4883281512132,11.1987310576086));
#26764=CARTESIAN_POINT('Ctrl Pts',(41.2968973614675,33.3748667810618,11.0971961933879));
#26765=CARTESIAN_POINT('Ctrl Pts',(41.2568614319233,33.2696766558841,11.));
#26766=CARTESIAN_POINT('Ctrl Pts',(40.2774792716873,34.9040806293113,11.2969997378715));
#26767=CARTESIAN_POINT('Ctrl Pts',(40.1574376536108,34.8925504003199,11.1987310576086));
#26768=CARTESIAN_POINT('Ctrl Pts',(40.0389585318563,34.8740199005147,11.0971961933879));
#26769=CARTESIAN_POINT('Ctrl Pts',(39.9284143148345,34.8528582802461,11.));
#26770=CARTESIAN_POINT('Origin',(41.0599821511772,34.4534158791985,11.));
#26771=CARTESIAN_POINT('',(40.9332180591367,33.7649895106091,24.2));
#26772=CARTESIAN_POINT('Origin',(41.0599821511772,34.4534158791985,24.2));
#26773=CARTESIAN_POINT('',(40.9332180591367,33.7649895106091,14.5));
#26774=CARTESIAN_POINT('Origin',(41.3363380414977,33.6162005901946,14.5));
#26775=CARTESIAN_POINT('',(41.7394580238587,33.4674116697801,24.2));
#26776=CARTESIAN_POINT('',(41.0787464646293,33.7112759382477,24.2));
#26777=CARTESIAN_POINT('',(41.7394580238587,33.4674116697801,11.5));
#26778=CARTESIAN_POINT('',(41.7394580238587,33.4674116697801,14.5));
#26779=CARTESIAN_POINT('Ctrl Pts',(41.7394580238587,33.4674116697801,11.5));
#26780=CARTESIAN_POINT('Ctrl Pts',(41.5533359473942,33.5361080977276,11.3977655520833));
#26781=CARTESIAN_POINT('Ctrl Pts',(41.3679200920551,33.6045438641267,11.2969997378715));
#26782=CARTESIAN_POINT('Origin',(42.6178210224504,31.9759771719264,14.5));
#26783=CARTESIAN_POINT('',(42.614150940502,32.0094411178763,11.2969997378715));
#26784=CARTESIAN_POINT('',(42.5709753191419,32.4031180656586,11.5));
#26785=CARTESIAN_POINT('Ctrl Pts',(42.614150940502,32.0094411178763,11.2969997378715));
#26786=CARTESIAN_POINT('Ctrl Pts',(42.5926041640387,32.2059054402286,11.3977655520829));
#26787=CARTESIAN_POINT('Ctrl Pts',(42.5709753191419,32.4031180656586,11.5));
#26788=CARTESIAN_POINT('',(42.5709753191419,32.4031180656586,24.2));
#26789=CARTESIAN_POINT('',(42.5709753191419,32.4031180656586,14.5));
#26790=CARTESIAN_POINT('',(42.6646667257588,31.5488362781942,24.2));
#26791=CARTESIAN_POINT('',(42.6477551837739,31.7030363573407,24.2));
#26792=CARTESIAN_POINT('',(42.6646667257588,31.5488362781942,11.5));
#26793=CARTESIAN_POINT('',(42.6646667257588,31.5488362781942,14.5));
#26794=CARTESIAN_POINT('Ctrl Pts',(42.6646667257588,31.5488362781942,11.5));
#26795=CARTESIAN_POINT('Ctrl Pts',(42.6426074344941,31.7499737298808,11.4654707447276));
#26796=CARTESIAN_POINT('Ctrl Pts',(42.614150940502,32.0094411178763,11.2969997378715));
#26797=CARTESIAN_POINT('Origin',(43.3633108984972,31.5052895228766,11.25));
#26798=CARTESIAN_POINT('',(43.1888334015084,30.827382742379,11.5));
#26799=CARTESIAN_POINT('Origin',(43.3633108984972,31.5052895228766,11.5));
#26800=CARTESIAN_POINT('',(43.6112843995965,30.6370046524817,11.2969997378715));
#26801=CARTESIAN_POINT('Ctrl Pts',(43.6112843995965,30.6370046524817,11.2969997378715));
#26802=CARTESIAN_POINT('Ctrl Pts',(43.3733097897213,30.7442482189004,11.4654707447276));
#26803=CARTESIAN_POINT('Ctrl Pts',(43.1888334015084,30.827382742379,11.5));
#26804=CARTESIAN_POINT('Ctrl Pts',(43.6112843995965,30.6370046524817,11.2969997378715));
#26805=CARTESIAN_POINT('Ctrl Pts',(43.5710559718872,30.523318198341,11.1987310576087));
#26806=CARTESIAN_POINT('Ctrl Pts',(43.5244132133966,30.412841346489,11.0971961933879));
#26807=CARTESIAN_POINT('Ctrl Pts',(43.4771371171594,30.3107002244375,11.));
#26808=CARTESIAN_POINT('Ctrl Pts',(42.614150940502,32.0094411178763,11.2969997378715));
#26809=CARTESIAN_POINT('Ctrl Pts',(42.4935974296579,32.0063126559227,11.1987310576087));
#26810=CARTESIAN_POINT('Ctrl Pts',(42.3741142947662,31.9960919812296,11.0971961933879));
#26811=CARTESIAN_POINT('Ctrl Pts',(42.2623631978924,31.9826930843766,11.));
#26812=CARTESIAN_POINT('Origin',(43.3633108984972,31.5052895228766,11.));
#26813=CARTESIAN_POINT('',(43.1888334015084,30.827382742379,24.2));
#26814=CARTESIAN_POINT('Origin',(43.3633108984972,31.5052895228766,24.2));
#26815=CARTESIAN_POINT('',(43.1888334015084,30.827382742379,14.5));
#26816=CARTESIAN_POINT('Origin',(43.5805924134327,30.6508360358314,14.5));
#26817=CARTESIAN_POINT('',(43.9723514253571,30.4742893292837,24.2));
#26818=CARTESIAN_POINT('',(43.3302604377194,30.7636484651835,24.2));
#26819=CARTESIAN_POINT('',(43.9723514253571,30.4742893292837,11.5));
#26820=CARTESIAN_POINT('',(43.9723514253571,30.4742893292837,14.5));
#26821=CARTESIAN_POINT('Ctrl Pts',(43.9723514253571,30.4742893292837,11.5));
#26822=CARTESIAN_POINT('Ctrl Pts',(43.7914747534882,30.5558016359257,11.397765552083));
#26823=CARTESIAN_POINT('Ctrl Pts',(43.6112843995965,30.6370046524817,11.2969997378715));
#26824=CARTESIAN_POINT('Origin',(44.74453756444,28.9252163854584,14.5));
#26825=CARTESIAN_POINT('',(44.7432107494939,28.9588548268927,11.2969997378715));
#26826=CARTESIAN_POINT('',(44.727601817449,29.3545845765144,11.5));
#26827=CARTESIAN_POINT('Ctrl Pts',(44.7432107494939,28.9588548268927,11.2969997378715));
#26828=CARTESIAN_POINT('Ctrl Pts',(44.7354211182387,29.156343599178,11.3977655520835));
#26829=CARTESIAN_POINT('Ctrl Pts',(44.727601817449,29.3545845765144,11.5));
#26830=CARTESIAN_POINT('',(44.727601817449,29.3545845765144,24.2));
#26831=CARTESIAN_POINT('',(44.727601817449,29.3545845765144,14.5));
#26832=CARTESIAN_POINT('',(44.7614733114311,28.4958481944023,24.2));
#26833=CARTESIAN_POINT('',(44.7553594188847,28.6508523394404,24.2));
#26834=CARTESIAN_POINT('',(44.7614733114311,28.4958481944023,11.5));
#26835=CARTESIAN_POINT('',(44.7614733114311,28.4958481944023,14.5));
#26836=CARTESIAN_POINT('Ctrl Pts',(44.7614733114311,28.4958481944023,11.5));
#26837=CARTESIAN_POINT('Ctrl Pts',(44.7534983948587,28.6980344637377,11.4654707447276));
#26838=CARTESIAN_POINT('Ctrl Pts',(44.7432107494939,28.9588548268927,11.2969997378715));
#26839=CARTESIAN_POINT('Origin',(45.4553779539844,28.4036725628998,11.25));
#26840=CARTESIAN_POINT('',(45.2340370888744,27.7395880641857,11.5));
#26841=CARTESIAN_POINT('Origin',(45.4553779539844,28.4036725628998,11.5));
#26842=CARTESIAN_POINT('',(45.6421789133341,27.5202050337906,11.2969997378715));
#26843=CARTESIAN_POINT('Ctrl Pts',(45.6421789133341,27.5202050337906,11.2969997378715));
#26844=CARTESIAN_POINT('Ctrl Pts',(45.4122649306731,27.6437876298971,11.4654707447276));
#26845=CARTESIAN_POINT('Ctrl Pts',(45.2340370888744,27.7395880641857,11.5));
#26846=CARTESIAN_POINT('Ctrl Pts',(45.6421789133341,27.5202050337906,11.2969997378715));
#26847=CARTESIAN_POINT('Ctrl Pts',(45.5941181138995,27.4096017073997,11.1987310576086));
#26848=CARTESIAN_POINT('Ctrl Pts',(45.5398824992087,27.3026476059642,11.0971961933879));
#26849=CARTESIAN_POINT('Ctrl Pts',(45.4855965606673,27.2040531083184,11.));
#26850=CARTESIAN_POINT('Ctrl Pts',(44.7432107494939,28.9588548268927,11.2969997378715));
#26851=CARTESIAN_POINT('Ctrl Pts',(44.6227326704691,28.9641433735292,11.1987310576086));
#26852=CARTESIAN_POINT('Ctrl Pts',(44.5028276322628,28.9622823180478,11.0971961933879));
#26853=CARTESIAN_POINT('Ctrl Pts',(44.390414095648,28.9567114226892,11.));
#26854=CARTESIAN_POINT('Origin',(45.4553779539844,28.4036725628998,11.));
#26855=CARTESIAN_POINT('',(45.2340370888744,27.7395880641857,24.2));
#26856=CARTESIAN_POINT('Origin',(45.4553779539844,28.4036725628998,24.2));
#26857=CARTESIAN_POINT('',(45.2340370888744,27.7395880641857,14.5));
#26858=CARTESIAN_POINT('Origin',(45.6125265198356,27.5361436893125,14.5));
#26859=CARTESIAN_POINT('',(45.9910159507968,27.3326993144394,24.2));
#26860=CARTESIAN_POINT('',(45.3706737374995,27.6661435891479,24.2));
#26861=CARTESIAN_POINT('',(45.9910159507968,27.3326993144394,11.5));
#26862=CARTESIAN_POINT('',(45.9910159507968,27.3326993144394,14.5));
#26863=CARTESIAN_POINT('Ctrl Pts',(45.9910159507968,27.3326993144394,11.5));
#26864=CARTESIAN_POINT('Ctrl Pts',(45.8162658964868,27.426630380012,11.3977655520824));
#26865=CARTESIAN_POINT('Ctrl Pts',(45.6421789133341,27.5202050337906,11.2969997378715));
#26866=CARTESIAN_POINT('Origin',(46.653263217121,25.7335348523128,14.5));
#26867=CARTESIAN_POINT('',(46.6542861332861,25.7671839061264,11.2969997378715));
#26868=CARTESIAN_POINT('',(46.6663199357044,26.1630385020257,11.5));
#26869=CARTESIAN_POINT('Ctrl Pts',(46.6542861332861,25.7671839061264,11.2969997378715));
#26870=CARTESIAN_POINT('Ctrl Pts',(46.6602915975398,25.964734982895,11.3977655520828));
#26871=CARTESIAN_POINT('Ctrl Pts',(46.6663199357044,26.1630385020257,11.5));
#26872=CARTESIAN_POINT('',(46.6663199357044,26.1630385020257,24.2));
#26873=CARTESIAN_POINT('',(46.6663199357044,26.1630385020257,14.5));
#26874=CARTESIAN_POINT('',(46.6402064985376,25.3040312025999,24.2));
#26875=CARTESIAN_POINT('',(46.6449200416998,25.459084248916,24.2));
#26876=CARTESIAN_POINT('',(46.6402064985376,25.3040312025999,11.5));
#26877=CARTESIAN_POINT('',(46.6402064985376,25.3040312025999,14.5));
#26878=CARTESIAN_POINT('Ctrl Pts',(46.6402064985376,25.3040312025999,11.5));
#26879=CARTESIAN_POINT('Ctrl Pts',(46.6463548096495,25.5062812584034,11.4654707447275));
#26880=CARTESIAN_POINT('Ctrl Pts',(46.6542861332861,25.7671839061264,11.2969997378715));
#26881=CARTESIAN_POINT('Origin',(47.3259909772385,25.1636757653237,11.25));
#26882=CARTESIAN_POINT('',(47.0588650944529,24.5166489013173,11.5));
#26883=CARTESIAN_POINT('Origin',(47.3259909772385,25.1636757653237,11.5));
#26884=CARTESIAN_POINT('',(47.4507093193416,24.2693297424963,11.2969997378715));
#26885=CARTESIAN_POINT('Ctrl Pts',(47.4507093193416,24.2693297424963,11.2969997378715));
#26886=CARTESIAN_POINT('Ctrl Pts',(47.2299760817075,24.4086492863048,11.4654707447276));
#26887=CARTESIAN_POINT('Ctrl Pts',(47.0588650944529,24.5166489013173,11.5));
#26888=CARTESIAN_POINT('Ctrl Pts',(47.4507093193416,24.2693297424963,11.2969997378714));
#26889=CARTESIAN_POINT('Ctrl Pts',(47.3950502955655,24.1623483921434,11.1987310576086));
#26890=CARTESIAN_POINT('Ctrl Pts',(47.3334860551377,24.0594381107558,11.0971961933879));
#26891=CARTESIAN_POINT('Ctrl Pts',(47.2724547499278,23.9648705799974,11.));
#26892=CARTESIAN_POINT('Ctrl Pts',(46.6542861332861,25.7671839061264,11.2969997378715));
#26893=CARTESIAN_POINT('Ctrl Pts',(46.5344704431712,25.7808636960853,11.1987310576086));
#26894=CARTESIAN_POINT('Ctrl Pts',(46.4147276669439,25.787371326691,11.0971961933879));
#26895=CARTESIAN_POINT('Ctrl Pts',(46.3021993580384,25.7896555736688,11.));
#26896=CARTESIAN_POINT('Origin',(47.3259909772385,25.1636757653237,11.));
#26897=CARTESIAN_POINT('',(47.0588650944529,24.5166489013173,24.2));
#26898=CARTESIAN_POINT('Origin',(47.3259909772385,25.1636757653237,24.2));
#26899=CARTESIAN_POINT('',(47.0588650944529,24.5166489013173,14.5));
#26900=CARTESIAN_POINT('Origin',(47.4222409819888,24.287298018663,14.5));
#26901=CARTESIAN_POINT('',(47.7856168695248,24.0579471360087,24.2));
#26902=CARTESIAN_POINT('',(47.1900456754746,24.4338520425371,24.2));
#26903=CARTESIAN_POINT('',(47.7856168695248,24.0579471360087,11.5));
#26904=CARTESIAN_POINT('',(47.7856168695248,24.0579471360087,14.5));
#26905=CARTESIAN_POINT('Ctrl Pts',(47.7856168695248,24.0579471360087,11.5));
#26906=CARTESIAN_POINT('Ctrl Pts',(47.6178447974735,24.1638393378018,11.3977655520823));
#26907=CARTESIAN_POINT('Ctrl Pts',(47.4507093193416,24.2693297424963,11.2969997378715));
#26908=CARTESIAN_POINT('Origin',(48.3346988609778,22.4164821240926,14.5));
#26909=CARTESIAN_POINT('',(48.3380665247094,22.4499778554777,11.2969997378715));
#26910=CARTESIAN_POINT('',(48.3776844341152,22.8440287338545,11.5));
#26911=CARTESIAN_POINT('Ctrl Pts',(48.3380665247094,22.4499778554777,11.2969997378715));
#26912=CARTESIAN_POINT('Ctrl Pts',(48.3578378264538,22.646628787743,11.397765552083));
#26913=CARTESIAN_POINT('Ctrl Pts',(48.3776844341152,22.8440287338545,11.5));
#26914=CARTESIAN_POINT('',(48.3776844341152,22.8440287338545,24.2));
#26915=CARTESIAN_POINT('',(48.3776844341152,22.8440287338545,14.5));
#26916=CARTESIAN_POINT('',(48.2917132878405,21.9889355143307,24.2));
#26917=CARTESIAN_POINT('',(48.3072313028027,22.1432820590691,24.2));
#26918=CARTESIAN_POINT('',(48.2917132878405,21.9889355143307,11.5));
#26919=CARTESIAN_POINT('',(48.2917132878405,21.9889355143307,14.5));
#26920=CARTESIAN_POINT('Ctrl Pts',(48.2917132878405,21.9889355143307,11.5));
#26921=CARTESIAN_POINT('Ctrl Pts',(48.3119548726829,22.1902640146607,11.4654707447276));
#26922=CARTESIAN_POINT('Ctrl Pts',(48.3380665247094,22.4499778554777,11.2969997378715));
#26923=CARTESIAN_POINT('Origin',(48.9660365296434,21.8010840688629,11.25));
#26924=CARTESIAN_POINT('',(48.6544270396318,21.1742670894066,11.5));
#26925=CARTESIAN_POINT('Origin',(48.9660365296434,21.8010840688629,11.5));
#26926=CARTESIAN_POINT('',(49.028064639274,20.9002167162411,11.2969997378715));
#26927=CARTESIAN_POINT('Ctrl Pts',(49.028064639274,20.9002167162411,11.2969997378715));
#26928=CARTESIAN_POINT('Ctrl Pts',(48.8175875368124,21.0545944569385,11.4654707447276));
#26929=CARTESIAN_POINT('Ctrl Pts',(48.6544270396318,21.1742670894066,11.5));
#26930=CARTESIAN_POINT('Ctrl Pts',(49.028064639274,20.9002167162411,11.2969997378715));
#26931=CARTESIAN_POINT('Ctrl Pts',(48.9650785563254,20.7973785443115,11.1987310576086));
#26932=CARTESIAN_POINT('Ctrl Pts',(48.8964856249514,20.699013451518,11.0971961933879));
#26933=CARTESIAN_POINT('Ctrl Pts',(48.8290062914572,20.608933611151,11.));
#26934=CARTESIAN_POINT('Ctrl Pts',(48.3380665247094,22.4499778554777,11.2969997378715));
#26935=CARTESIAN_POINT('Ctrl Pts',(48.2194969535028,22.4719822421975,11.1987310576086));
#26936=CARTESIAN_POINT('Ctrl Pts',(48.1004998140235,22.4868268543681,11.0971961933879));
#26937=CARTESIAN_POINT('Ctrl Pts',(47.9884049594373,22.4969551150606,11.));
#26938=CARTESIAN_POINT('Origin',(48.9660365296434,21.8010840688629,11.));
#26939=CARTESIAN_POINT('',(48.6544270396318,21.1742670894066,24.2));
#26940=CARTESIAN_POINT('Origin',(48.9660365296434,21.8010840688629,24.2));
#26941=CARTESIAN_POINT('',(48.6544270396318,21.1742670894066,14.5));
#26942=CARTESIAN_POINT('Origin',(49.0009190529448,20.9201270734172,14.5));
#26943=CARTESIAN_POINT('',(49.3474110662579,20.6659870574277,24.2));
#26944=CARTESIAN_POINT('',(48.7795124544456,21.0825212248573,24.2));
#26945=CARTESIAN_POINT('',(49.3474110662579,20.6659870574277,11.5));
#26946=CARTESIAN_POINT('',(49.3474110662579,20.6659870574277,14.5));
#26947=CARTESIAN_POINT('Ctrl Pts',(49.3474110662579,20.6659870574277,11.5));
#26948=CARTESIAN_POINT('Ctrl Pts',(49.1874343451369,20.7833244992778,11.3977655520829));
#26949=CARTESIAN_POINT('Ctrl Pts',(49.028064639274,20.9002167162411,11.2969997378715));
#26950=CARTESIAN_POINT('Origin',(49.7806527105708,18.9902185482608,14.5));
#26951=CARTESIAN_POINT('',(49.7863487149497,19.0233977693811,11.2969997378715));
#26952=CARTESIAN_POINT('',(49.8533577168707,19.4137251539658,11.5));
#26953=CARTESIAN_POINT('Ctrl Pts',(49.7863487149497,19.0233977693811,11.2969997378715));
#26954=CARTESIAN_POINT('Ctrl Pts',(49.8197895303901,19.2181904935678,11.3977655520829));
#26955=CARTESIAN_POINT('Ctrl Pts',(49.8533577168707,19.4137251539658,11.5));
#26956=CARTESIAN_POINT('',(49.8533577168707,19.4137251539658,24.2));
#26957=CARTESIAN_POINT('',(49.8533577168707,19.4137251539658,14.5));
#26958=CARTESIAN_POINT('',(49.707947704271,18.5667119425558,24.2));
#26959=CARTESIAN_POINT('',(49.7341945888243,18.7196000248653,24.2));
#26960=CARTESIAN_POINT('',(49.707947704271,18.5667119425558,11.5));
#26961=CARTESIAN_POINT('',(49.707947704271,18.5667119425558,14.5));
#26962=CARTESIAN_POINT('Ctrl Pts',(49.707947704271,18.5667119425558,11.5));
#26963=CARTESIAN_POINT('Ctrl Pts',(49.7421839478772,18.7661380351961,11.4654707447276));
#26964=CARTESIAN_POINT('Ctrl Pts',(49.7863487149497,19.0233977693811,11.2969997378715));
#26965=CARTESIAN_POINT('Origin',(50.3675244741247,18.3322796822558,11.25));
#26966=CARTESIAN_POINT('',(50.0129495069995,17.7287263766662,11.5));
#26967=CARTESIAN_POINT('Origin',(50.3675244741247,18.3322796822558,11.5));
#26968=CARTESIAN_POINT('',(50.3665601565676,17.4292799350267,11.2969997378715));
#26969=CARTESIAN_POINT('Ctrl Pts',(50.3665601565676,17.4292799350267,11.2969997378715));
#26970=CARTESIAN_POINT('Ctrl Pts',(50.1673646125648,17.5979637597785,11.4654707447276));
#26971=CARTESIAN_POINT('Ctrl Pts',(50.0129495069995,17.7287263766662,11.5));
#26972=CARTESIAN_POINT('Ctrl Pts',(50.3665601565676,17.4292799350267,11.2969997378715));
#26973=CARTESIAN_POINT('Ctrl Pts',(50.2965538763113,17.3310859587567,11.1987310576086));
#26974=CARTESIAN_POINT('Ctrl Pts',(50.2212664318579,17.2377452794019,11.0971961933879));
#26975=CARTESIAN_POINT('Ctrl Pts',(50.1476678226092,17.1525919893539,11.));
#26976=CARTESIAN_POINT('Ctrl Pts',(49.7863487149497,19.0233977693811,11.2969997378715));
#26977=CARTESIAN_POINT('Ctrl Pts',(49.6696029216838,19.0536195497014,11.1987310576086));
#26978=CARTESIAN_POINT('Ctrl Pts',(49.5519311610546,19.0767288219785,11.0971961933879));
#26979=CARTESIAN_POINT('Ctrl Pts',(49.4408158756514,19.0946517525179,11.));
#26980=CARTESIAN_POINT('Origin',(50.3675244741247,18.3322796822558,11.));
#26981=CARTESIAN_POINT('',(50.0129495069995,17.7287263766662,24.2));
#26982=CARTESIAN_POINT('Origin',(50.3675244741247,18.3322796822558,24.2));
#26983=CARTESIAN_POINT('',(50.0129495069995,17.7287263766662,14.5));
#26984=CARTESIAN_POINT('Origin',(50.34086957183,17.4510353719535,14.5));
#26985=CARTESIAN_POINT('',(50.6687896366606,17.1733443672407,24.2));
#26986=CARTESIAN_POINT('',(50.131330352038,17.6284784829776,24.2));
#26987=CARTESIAN_POINT('',(50.6687896366606,17.1733443672407,11.5));
#26988=CARTESIAN_POINT('',(50.6687896366606,17.1733443672407,14.5));
#26989=CARTESIAN_POINT('Ctrl Pts',(50.6687896366606,17.1733443672407,11.5));
#26990=CARTESIAN_POINT('Ctrl Pts',(50.5173876569737,17.3015553929261,11.3977655520831));
#26991=CARTESIAN_POINT('Ctrl Pts',(50.3665601565676,17.4292799350267,11.2969997378715));
#26992=CARTESIAN_POINT('Origin',(50.9840802240917,15.4714365365517,14.5));
#26993=CARTESIAN_POINT('',(50.9920768187572,15.5041376015772,11.2969997378715));
#26994=CARTESIAN_POINT('',(51.0861504520718,15.8888398565875,11.5));
#26995=CARTESIAN_POINT('Ctrl Pts',(50.9920768187572,15.5041376015772,11.2969997378715));
#26996=CARTESIAN_POINT('Ctrl Pts',(51.0390242276023,15.6961231071139,11.3977655520831));
#26997=CARTESIAN_POINT('Ctrl Pts',(51.0861504520718,15.8888398565875,11.5));
#26998=CARTESIAN_POINT('',(51.0861504520718,15.8888398565875,24.2));
#26999=CARTESIAN_POINT('',(51.0861504520718,15.8888398565875,14.5));
#27000=CARTESIAN_POINT('',(50.8820099961117,15.054033216516,24.2));
#27001=CARTESIAN_POINT('',(50.9188578780728,15.204717981028,24.2));
#27002=CARTESIAN_POINT('',(50.8820099961117,15.054033216516,11.5));
#27003=CARTESIAN_POINT('',(50.8820099961117,15.054033216516,14.5));
#27004=CARTESIAN_POINT('Ctrl Pts',(50.8820099961117,15.054033216516,11.5));
#27005=CARTESIAN_POINT('Ctrl Pts',(50.9300741029444,15.2505853175896,11.4654707447276));
#27006=CARTESIAN_POINT('Ctrl Pts',(50.9920768187572,15.5041376015772,11.2969997378715));
#27007=CARTESIAN_POINT('Origin',(51.5236269022939,14.7741622717912,11.25));
#27008=CARTESIAN_POINT('',(51.1278139116531,14.1968130911041,11.5));
#27009=CARTESIAN_POINT('Origin',(51.5236269022939,14.7741622717912,11.5));
#27010=CARTESIAN_POINT('',(51.4596748556074,13.8734294539541,11.2969997378715));
#27011=CARTESIAN_POINT('Ctrl Pts',(51.4596748556075,13.8734294539541,11.2969997378715));
#27012=CARTESIAN_POINT('Ctrl Pts',(51.2727313307305,14.0555975521219,11.4654707447276));
#27013=CARTESIAN_POINT('Ctrl Pts',(51.1278139116531,14.1968130911041,11.5));
#27014=CARTESIAN_POINT('Ctrl Pts',(51.4596748556074,13.8734294539541,11.2969997378715));
#27015=CARTESIAN_POINT('Ctrl Pts',(51.3829894416038,13.7803580645257,11.1987310576087));
#27016=CARTESIAN_POINT('Ctrl Pts',(51.3013742769325,13.6924965450168,11.0971961933879));
#27017=CARTESIAN_POINT('Ctrl Pts',(51.2220149569554,13.6126846635571,11.));
#27018=CARTESIAN_POINT('Ctrl Pts',(50.9920768187572,15.5041376015772,11.2969997378715));
#27019=CARTESIAN_POINT('Ctrl Pts',(50.8777235772014,15.5424295380224,11.1987310576087));
#27020=CARTESIAN_POINT('Ctrl Pts',(50.7619504804118,15.5736908843544,11.0971961933879));
#27021=CARTESIAN_POINT('Ctrl Pts',(50.6523561066928,15.5993211660246,11.));
#27022=CARTESIAN_POINT('Origin',(51.5236269022939,14.7741622717912,11.));
#27023=CARTESIAN_POINT('',(51.1278139116531,14.1968130911041,24.2));
#27024=CARTESIAN_POINT('Origin',(51.5236269022939,14.7741622717912,24.2));
#27025=CARTESIAN_POINT('',(51.1278139116531,14.1968130911041,14.5));
#27026=CARTESIAN_POINT('Origin',(51.9391184236626,11.8772792412203,14.5));
#27027=CARTESIAN_POINT('',(51.8081802498931,11.4680127538715,11.0622545443403));
#27028=CARTESIAN_POINT('',(52.0700565974321,12.286545728569,11.5));
#27029=CARTESIAN_POINT('Ctrl Pts',(51.8081802498931,11.4680127538715,11.0622545443403));
#27030=CARTESIAN_POINT('Ctrl Pts',(51.9385805447408,11.8755980216752,11.2776618075205));
#27031=CARTESIAN_POINT('Ctrl Pts',(52.0700565974321,12.286545728569,11.5));
#27032=CARTESIAN_POINT('',(52.0700565974321,12.286545728569,24.2));
#27033=CARTESIAN_POINT('',(52.0700565974321,12.286545728569,14.5));
#27034=CARTESIAN_POINT('',(51.8081802498931,11.4680127538716,24.2));
#27035=CARTESIAN_POINT('',(51.8554496100851,11.6157600795601,24.2));
#27036=CARTESIAN_POINT('',(51.8081802498931,11.4680127538716,14.5));
#27037=CARTESIAN_POINT('Origin',(0.,0.,14.5));
#27038=CARTESIAN_POINT('',(51.7433149571623,13.5970348695554,11.5));
#27039=CARTESIAN_POINT('Origin',(0.,0.,11.5));
#27040=CARTESIAN_POINT('',(51.7433149571623,13.5970348695554,24.2));
#27041=CARTESIAN_POINT('',(51.7433149571623,13.5970348695554,14.5));
#27042=CARTESIAN_POINT('Origin',(0.,0.,24.2));
#27043=CARTESIAN_POINT('Origin',(0.,0.,11.25));
#27044=CARTESIAN_POINT('Ctrl Pts',(51.766094205967,11.3697621197168,11.));
#27045=CARTESIAN_POINT('Ctrl Pts',(51.7780926618965,11.4049882694565,11.0192759649605));
#27046=CARTESIAN_POINT('Ctrl Pts',(51.7924945631287,11.4379662231208,11.0404458048696));
#27047=CARTESIAN_POINT('Ctrl Pts',(51.8081802498931,11.4680127538714,11.0622545443403));
#27048=CARTESIAN_POINT('Ctrl Pts',(51.7433149571623,13.5970348695554,11.5));
#27049=CARTESIAN_POINT('Ctrl Pts',(51.6012253341355,13.7354948478468,11.3977655520831));
#27050=CARTESIAN_POINT('Ctrl Pts',(51.4596748556074,13.8734294539541,11.2969997378715));
#27051=CARTESIAN_POINT('Origin',(51.4355644344077,13.8969239803297,14.5));
#27052=CARTESIAN_POINT('',(51.238913447339,14.0885515659373,24.2));
#27053=CARTESIAN_POINT('Origin',(33.443838774836,41.4759138875076,14.5));
#27054=CARTESIAN_POINT('',(33.8690845744085,41.4141897191236,24.2));
#27055=CARTESIAN_POINT('',(33.0185929752635,41.5376380558916,24.2));
#27056=CARTESIAN_POINT('',(33.1721089155843,41.5153553108074,24.2));
#27057=CARTESIAN_POINT('',(33.8690845744085,41.4141897191236,11.5));
#27058=CARTESIAN_POINT('',(33.8690845744085,41.4141897191236,14.5));
#27059=CARTESIAN_POINT('',(33.0185929752634,41.5376380558916,11.0622545443402));
#27060=CARTESIAN_POINT('Ctrl Pts',(33.8690845744085,41.4141897191236,11.5));
#27061=CARTESIAN_POINT('Ctrl Pts',(33.4420919141158,41.4761674432754,11.2776618075192));
#27062=CARTESIAN_POINT('Ctrl Pts',(33.0185929752634,41.5376380558916,11.0622545443402));
#27063=CARTESIAN_POINT('',(33.0185929752635,41.5376380558916,14.5));
#27064=CARTESIAN_POINT('Origin',(0.,0.,11.25));
#27065=CARTESIAN_POINT('',(34.9037103045182,40.546035650582,11.5));
#27066=CARTESIAN_POINT('Origin',(0.,0.,11.5));
#27067=CARTESIAN_POINT('',(35.0277924748111,40.1699382050837,11.2969997378715));
#27068=CARTESIAN_POINT('Ctrl Pts',(35.0277924748111,40.1699382050837,11.2969997378715));
#27069=CARTESIAN_POINT('Ctrl Pts',(34.9658693176643,40.3576294838962,11.3977655520829));
#27070=CARTESIAN_POINT('Ctrl Pts',(34.9037103045182,40.546035650582,11.5));
#27071=CARTESIAN_POINT('Ctrl Pts',(35.0277924748111,40.1699382050837,11.2969997378715));
#27072=CARTESIAN_POINT('Ctrl Pts',(34.9105237912333,40.1418136232562,11.1987310576086));
#27073=CARTESIAN_POINT('Ctrl Pts',(34.7957766472675,40.1069743542277,11.0971961933879));
#27074=CARTESIAN_POINT('Ctrl Pts',(34.6892533672809,40.0706338959167,11.));
#27075=CARTESIAN_POINT('Ctrl Pts',(33.0185929752633,41.5376380558916,11.0622545443403));
#27076=CARTESIAN_POINT('Ctrl Pts',(32.9847111798176,41.5367113861579,11.0404458048696));
#27077=CARTESIAN_POINT('Ctrl Pts',(32.948757413446,41.5382236264416,11.0192759649605));
#27078=CARTESIAN_POINT('Ctrl Pts',(32.9118365829004,41.5428816133457,11.));
#27079=CARTESIAN_POINT('Origin',(0.,0.,14.5));
#27080=CARTESIAN_POINT('',(34.9037103045182,40.546035650582,24.2));
#27081=CARTESIAN_POINT('Origin',(0.,0.,24.2));
#27082=CARTESIAN_POINT('',(34.9037103045182,40.546035650582,14.5));
#27083=CARTESIAN_POINT('Origin',(35.0383399022473,40.137968579585,14.5));
#27084=CARTESIAN_POINT('',(35.1729694999764,39.729901508588,24.2));
#27085=CARTESIAN_POINT('',(35.1243675165795,39.8772158387497,24.2));
#27086=CARTESIAN_POINT('',(35.1729694999764,39.729901508588,11.5));
#27087=CARTESIAN_POINT('',(35.1729694999764,39.729901508588,14.5));
#27088=CARTESIAN_POINT('Ctrl Pts',(35.1729694999764,39.729901508588,11.5));
#27089=CARTESIAN_POINT('Ctrl Pts',(35.1095734294849,39.9220572398279,11.4654707447276));
#27090=CARTESIAN_POINT('Ctrl Pts',(35.0277924748111,40.1699382050837,11.2969997378715));
#27091=CARTESIAN_POINT('Origin',(36.2555847625695,39.0419563844502,14.5));
#27092=CARTESIAN_POINT('',(36.6754890244158,38.9507189255854,24.2));
#27093=CARTESIAN_POINT('',(35.8356805007232,39.1331938433149,24.2));
#27094=CARTESIAN_POINT('',(35.9872681182067,39.1002566472175,24.2));
#27095=CARTESIAN_POINT('',(36.6754890244158,38.9507189255854,11.5));
#27096=CARTESIAN_POINT('',(36.6754890244158,38.9507189255854,14.5));
#27097=CARTESIAN_POINT('',(36.288481761496,39.0348084727497,11.2969997378715));
#27098=CARTESIAN_POINT('Ctrl Pts',(36.6754890244158,38.9507189255854,11.5));
#27099=CARTESIAN_POINT('Ctrl Pts',(36.4816175803026,38.9928436180797,11.3977655520832));
#27100=CARTESIAN_POINT('Ctrl Pts',(36.288481761496,39.0348084727497,11.2969997378715));
#27101=CARTESIAN_POINT('',(35.8356805007232,39.1331938433149,11.5));
#27102=CARTESIAN_POINT('Ctrl Pts',(36.288481761496,39.0348084727497,11.2969997378715));
#27103=CARTESIAN_POINT('Ctrl Pts',(36.0334102765875,39.0902308064254,11.4654707447276));
#27104=CARTESIAN_POINT('Ctrl Pts',(35.8356805007232,39.1331938433149,11.5));
#27105=CARTESIAN_POINT('',(35.8356805007232,39.1331938433149,14.5));
#27106=CARTESIAN_POINT('Origin',(0.,0.,11.25));
#27107=CARTESIAN_POINT('',(37.6470350917587,38.0125077941444,11.5));
#27108=CARTESIAN_POINT('Origin',(0.,0.,11.5));
#27109=CARTESIAN_POINT('',(37.8587077455022,37.1795791419029,11.0622545443403));
#27110=CARTESIAN_POINT('Ctrl Pts',(37.8587077455022,37.1795791419029,11.0622545443403));
#27111=CARTESIAN_POINT('Ctrl Pts',(37.753306182059,37.5943326805875,11.277661807521));
#27112=CARTESIAN_POINT('Ctrl Pts',(37.6470350917587,38.0125077941444,11.5));
#27113=CARTESIAN_POINT('Ctrl Pts',(37.8750816598377,37.0739556732301,11.));
#27114=CARTESIAN_POINT('Ctrl Pts',(37.8665899121936,37.1101873553899,11.0192759649605));
#27115=CARTESIAN_POINT('Ctrl Pts',(37.861327764173,37.1457860911145,11.0404458048696));
#27116=CARTESIAN_POINT('Ctrl Pts',(37.8587077455022,37.1795791419029,11.0622545443404));
#27117=CARTESIAN_POINT('Ctrl Pts',(36.288481761496,39.0348084727497,11.2969997378715));
#27118=CARTESIAN_POINT('Ctrl Pts',(36.2727691643543,38.9152423799721,11.1987310576087));
#27119=CARTESIAN_POINT('Ctrl Pts',(36.2501150911098,38.7974821376142,11.0971961933879));
#27120=CARTESIAN_POINT('Ctrl Pts',(36.2251084243911,38.6877437910394,11.));
#27121=CARTESIAN_POINT('Origin',(0.,0.,14.5));
#27122=CARTESIAN_POINT('',(37.6470350917587,38.0125077941444,24.2));
#27123=CARTESIAN_POINT('Origin',(0.,0.,24.2));
#27124=CARTESIAN_POINT('',(37.6470350917587,38.0125077941444,14.5));
#27125=CARTESIAN_POINT('Origin',(38.8906971857384,36.4177903943714,14.5));
#27126=CARTESIAN_POINT('',(38.4781801929734,36.5380966439885,11.0622545443404));
#27127=CARTESIAN_POINT('',(38.4781801929734,36.5380966439885,24.2));
#27128=CARTESIAN_POINT('',(38.4781801929734,36.5380966439885,14.5));
#27129=CARTESIAN_POINT('',(39.3032141785034,36.2974841447543,24.2));
#27130=CARTESIAN_POINT('',(38.6271009679847,36.4946654635865,24.2));
#27131=CARTESIAN_POINT('',(39.3032141785034,36.2974841447543,11.5));
#27132=CARTESIAN_POINT('',(39.3032141785034,36.2974841447543,14.5));
#27133=CARTESIAN_POINT('Ctrl Pts',(39.3032141785034,36.2974841447543,11.5));
#27134=CARTESIAN_POINT('Ctrl Pts',(39.0288731206038,36.3774928337799,11.352740724575));
#27135=CARTESIAN_POINT('Ctrl Pts',(38.7538500369047,36.4577004284687,11.2067970124648));
#27136=CARTESIAN_POINT('Ctrl Pts',(38.4781801929734,36.5380966439885,11.0622545443404));
#27137=CARTESIAN_POINT('Origin',(0.,0.,11.25));
#27138=CARTESIAN_POINT('Ctrl Pts',(38.3731925086332,36.5581467896744,11.));
#27139=CARTESIAN_POINT('Ctrl Pts',(38.4091053726145,36.548395853148,11.0192757561174));
#27140=CARTESIAN_POINT('Ctrl Pts',(38.4444995059675,36.54189438867,11.0404460254343));
#27141=CARTESIAN_POINT('Ctrl Pts',(38.4781801929734,36.5380966439885,11.0622545443404));
#27142=CARTESIAN_POINT('Origin',(0.,0.,11.5));
#27143=CARTESIAN_POINT('Origin',(0.,0.,11.25));
#27144=CARTESIAN_POINT('Origin',(0.,0.,11.5));
#27145=CARTESIAN_POINT('Origin',(0.,0.,11.25));
#27146=CARTESIAN_POINT('Origin',(0.,0.,11.5));
#27147=CARTESIAN_POINT('Origin',(0.,0.,11.25));
#27148=CARTESIAN_POINT('Origin',(0.,0.,11.5));
#27149=CARTESIAN_POINT('Origin',(0.,0.,11.25));
#27150=CARTESIAN_POINT('Origin',(0.,0.,11.5));
#27151=CARTESIAN_POINT('Origin',(0.,0.,11.25));
#27152=CARTESIAN_POINT('Origin',(0.,0.,11.5));
#27153=CARTESIAN_POINT('Origin',(0.,0.,11.25));
#27154=CARTESIAN_POINT('Origin',(0.,0.,11.5));
#27155=CARTESIAN_POINT('Origin',(0.,0.,14.5));
#27156=CARTESIAN_POINT('Origin',(0.,0.,24.2));
#27157=CARTESIAN_POINT('Origin',(0.,0.,14.5));
#27158=CARTESIAN_POINT('Origin',(0.,0.,24.2));
#27159=CARTESIAN_POINT('Origin',(0.,0.,14.5));
#27160=CARTESIAN_POINT('Origin',(0.,0.,24.2));
#27161=CARTESIAN_POINT('Origin',(0.,0.,14.5));
#27162=CARTESIAN_POINT('Origin',(0.,0.,24.2));
#27163=CARTESIAN_POINT('Origin',(0.,0.,14.5));
#27164=CARTESIAN_POINT('Origin',(0.,0.,24.2));
#27165=CARTESIAN_POINT('Origin',(0.,0.,14.5));
#27166=CARTESIAN_POINT('Origin',(0.,0.,24.2));
#27167=CARTESIAN_POINT('Origin',(0.,0.,14.5));
#27168=CARTESIAN_POINT('Origin',(0.,0.,24.2));
#27169=CARTESIAN_POINT('Origin',(37.7528714186305,37.5960434680237,14.5));
#27170=CARTESIAN_POINT('',(37.8587077455022,37.1795791419031,24.2));
#27171=CARTESIAN_POINT('',(37.8205002822982,37.3299249247391,24.2));
#27172=CARTESIAN_POINT('',(37.8587077455022,37.1795791419031,14.5));
#27173=CARTESIAN_POINT('Origin',(35.8654005008348,39.8325626455883,11.25));
#27174=CARTESIAN_POINT('Origin',(35.8654005008348,39.8325626455883,11.5));
#27175=CARTESIAN_POINT('Origin',(38.5566132981517,37.2336886566023,11.));
#27176=CARTESIAN_POINT('Origin',(38.5566132981517,37.2336886566023,24.2));
#27177=CARTESIAN_POINT('Origin',(35.8654005008348,39.8325626455883,11.));
#27178=CARTESIAN_POINT('Origin',(35.8654005008348,39.8325626455883,24.2));
#27179=CARTESIAN_POINT('Origin',(4.75410644754494,53.0673181599239,14.5));
#27180=CARTESIAN_POINT('',(4.72678212511286,53.0869825079594,11.2969997378715));
#27181=CARTESIAN_POINT('',(4.4053330087579,53.318318063138,11.5));
#27182=CARTESIAN_POINT('Ctrl Pts',(4.72678212511286,53.0869825079594,11.2969997378715));
#27183=CARTESIAN_POINT('Ctrl Pts',(4.56636307296556,53.2024304236685,11.3977655520829));
#27184=CARTESIAN_POINT('Ctrl Pts',(4.4053330087579,53.318318063138,11.5));
#27185=CARTESIAN_POINT('',(4.4053330087579,53.318318063138,24.2));
#27186=CARTESIAN_POINT('',(4.40533300875789,53.318318063138,14.5));
#27187=CARTESIAN_POINT('',(5.102879886332,52.8163182567097,24.2));
#27188=CARTESIAN_POINT('',(4.97697086508332,52.9069305242525,24.2));
#27189=CARTESIAN_POINT('',(5.102879886332,52.8163182567097,11.5));
#27190=CARTESIAN_POINT('',(5.10287988633199,52.8163182567097,14.5));
#27191=CARTESIAN_POINT('Ctrl Pts',(5.102879886332,52.8163182567097,11.5));
#27192=CARTESIAN_POINT('Ctrl Pts',(4.93864508296158,52.9345122335611,11.4654707447275));
#27193=CARTESIAN_POINT('Ctrl Pts',(4.72678212511286,53.0869825079594,11.2969997378715));
#27194=CARTESIAN_POINT('Origin',(5.60272563114623,53.3063735917395,11.25));
#27195=CARTESIAN_POINT('',(5.98976031387286,52.7231033676009,11.5));
#27196=CARTESIAN_POINT('Origin',(5.60272563114623,53.3063735917395,11.5));
#27197=CARTESIAN_POINT('',(6.413913698772,52.9096578341174,11.2969997378715));
#27198=CARTESIAN_POINT('Ctrl Pts',(6.413913698772,52.9096578341174,11.2969997378715));
#27199=CARTESIAN_POINT('Ctrl Pts',(6.17498010231834,52.8045681868194,11.4654707447277));
#27200=CARTESIAN_POINT('Ctrl Pts',(5.98976031387286,52.7231033676009,11.5));
#27201=CARTESIAN_POINT('Ctrl Pts',(6.413913698772,52.9096578341174,11.2969997378716));
#27202=CARTESIAN_POINT('Ctrl Pts',(6.47148112666752,52.8036912002343,11.1987310576087));
#27203=CARTESIAN_POINT('Ctrl Pts',(6.5223713301853,52.6951054327476,11.0971961933879));
#27204=CARTESIAN_POINT('Ctrl Pts',(6.56664309356487,52.5916266955277,11.));
#27205=CARTESIAN_POINT('Ctrl Pts',(4.72678212511286,53.0869825079594,11.2969997378714));
#27206=CARTESIAN_POINT('Ctrl Pts',(4.64844098161554,52.9953004405385,11.1987310576086));
#27207=CARTESIAN_POINT('Ctrl Pts',(4.57608660062689,52.899668200857,11.0971961933879));
#27208=CARTESIAN_POINT('Ctrl Pts',(4.51126784227787,52.8076553394982,11.));
#27209=CARTESIAN_POINT('Origin',(5.60272563114623,53.3063735917395,11.));
#27210=CARTESIAN_POINT('',(5.98976031387286,52.7231033676009,24.2));
#27211=CARTESIAN_POINT('Origin',(5.60272563114623,53.3063735917395,24.2));
#27212=CARTESIAN_POINT('',(5.98976031387286,52.7231033676009,14.5));
#27213=CARTESIAN_POINT('Origin',(6.38309803049426,52.8961042453437,14.5));
#27214=CARTESIAN_POINT('',(6.77643574711566,53.0691051230866,24.2));
#27215=CARTESIAN_POINT('',(6.13175727067173,52.785557582198,24.2));
#27216=CARTESIAN_POINT('',(6.77643574711566,53.0691051230866,11.5));
#27217=CARTESIAN_POINT('',(6.77643574711566,53.0691051230866,14.5));
#27218=CARTESIAN_POINT('Ctrl Pts',(6.77643574711566,53.0691051230866,11.5));
#27219=CARTESIAN_POINT('Ctrl Pts',(6.59483018109884,52.989229939507,11.3977655520833));
#27220=CARTESIAN_POINT('Ctrl Pts',(6.413913698772,52.9096578341174,11.2969997378715));
#27221=CARTESIAN_POINT('Origin',(8.44431466907315,52.6064191384554,14.5));
#27222=CARTESIAN_POINT('',(8.41842862289464,52.6279416335077,11.2969997378715));
#27223=CARTESIAN_POINT('',(8.11389969301204,52.8811368237459,11.5));
#27224=CARTESIAN_POINT('Ctrl Pts',(8.41842862289464,52.6279416335077,11.2969997378715));
#27225=CARTESIAN_POINT('Ctrl Pts',(8.26645358299653,52.7542985912959,11.397765552083));
#27226=CARTESIAN_POINT('Ctrl Pts',(8.11389969301204,52.8811368237459,11.5));
#27227=CARTESIAN_POINT('',(8.11389969301204,52.8811368237459,24.2));
#27228=CARTESIAN_POINT('',(8.11389969301204,52.8811368237459,14.5));
#27229=CARTESIAN_POINT('',(8.77472964513427,52.3317014531649,24.2));
#27230=CARTESIAN_POINT('',(8.65544812419494,52.430875963113,24.2));
#27231=CARTESIAN_POINT('',(8.77472964513427,52.3317014531649,11.5));
#27232=CARTESIAN_POINT('',(8.77472964513427,52.3317014531649,14.5));
#27233=CARTESIAN_POINT('Ctrl Pts',(8.77472964513427,52.3317014531649,11.5));
#27234=CARTESIAN_POINT('Ctrl Pts',(8.6191397045334,52.4610639561783,11.4654707447276));
#27235=CARTESIAN_POINT('Ctrl Pts',(8.41842862289464,52.6279416335077,11.2969997378715));
#27236=CARTESIAN_POINT('Origin',(9.30754232294747,52.7856955614544,11.25));
#27237=CARTESIAN_POINT('',(9.65294733456355,52.1768479795831,11.5));
#27238=CARTESIAN_POINT('Origin',(9.30754232294747,52.7856955614544,11.5));
#27239=CARTESIAN_POINT('',(10.0890808848803,52.3333605643381,11.2969997378715));
#27240=CARTESIAN_POINT('Ctrl Pts',(10.0890808848803,52.3333605643381,11.2969997378715));
#27241=CARTESIAN_POINT('Ctrl Pts',(9.84339863543633,52.2451940752868,11.4654707447276));
#27242=CARTESIAN_POINT('Ctrl Pts',(9.65294733456355,52.1768479795831,11.5));
#27243=CARTESIAN_POINT('Ctrl Pts',(10.0890808848803,52.3333605643381,11.2969997378715));
#27244=CARTESIAN_POINT('Ctrl Pts',(10.1391162227005,52.2236363590767,11.1987310576086));
#27245=CARTESIAN_POINT('Ctrl Pts',(10.1823079000016,52.1117651799167,11.0971961933879));
#27246=CARTESIAN_POINT('Ctrl Pts',(10.2192535077747,52.0054502696,11.));
#27247=CARTESIAN_POINT('Ctrl Pts',(8.41842862289465,52.6279416335078,11.2969997378715));
#27248=CARTESIAN_POINT('Ctrl Pts',(8.33388289675663,52.5419477009147,11.1987310576086));
#27249=CARTESIAN_POINT('Ctrl Pts',(8.25503379958712,52.4515956030403,11.0971961933879));
#27250=CARTESIAN_POINT('Ctrl Pts',(8.18395444372813,52.3643284084021,11.));
#27251=CARTESIAN_POINT('Origin',(9.30754232294747,52.7856955614544,11.));
#27252=CARTESIAN_POINT('',(9.65294733456355,52.1768479795831,24.2));
#27253=CARTESIAN_POINT('Origin',(9.30754232294747,52.7856955614544,24.2));
#27254=CARTESIAN_POINT('',(9.65294733456355,52.1768479795831,14.5));
#27255=CARTESIAN_POINT('Origin',(10.0573948314625,52.3219895837806,14.5));
#27256=CARTESIAN_POINT('',(10.4618423283614,52.4671311879781,24.2));
#27257=CARTESIAN_POINT('',(9.79895497969307,52.2292448518636,24.2));
#27258=CARTESIAN_POINT('',(10.4618423283614,52.4671311879781,11.5));
#27259=CARTESIAN_POINT('',(10.4618423283614,52.4671311879781,14.5));
#27260=CARTESIAN_POINT('Ctrl Pts',(10.4618423283614,52.4671311879781,11.5));
#27261=CARTESIAN_POINT('Ctrl Pts',(10.2751073332288,52.4001187402286,11.3977655520829));
#27262=CARTESIAN_POINT('Ctrl Pts',(10.0890808848803,52.3333605643381,11.2969997378715));
#27263=CARTESIAN_POINT('Origin',(12.0933830383533,51.8892269309231,14.5));
#27264=CARTESIAN_POINT('',(12.0690613826432,51.9125027175599,11.2969997378715));
#27265=CARTESIAN_POINT('',(11.7829362735685,52.1863240013418,11.5));
#27266=CARTESIAN_POINT('Ctrl Pts',(12.0690613826432,51.9125027175599,11.2969997378715));
#27267=CARTESIAN_POINT('Ctrl Pts',(11.926270762113,52.0491531190295,11.3977655520827));
#27268=CARTESIAN_POINT('Ctrl Pts',(11.7829362735685,52.1863240013418,11.5));
#27269=CARTESIAN_POINT('',(11.7829362735685,52.1863240013418,24.2));
#27270=CARTESIAN_POINT('',(11.7829362735685,52.1863240013418,14.5));
#27271=CARTESIAN_POINT('',(12.4038298031382,51.5921298605044,24.2));
#27272=CARTESIAN_POINT('',(12.2917569100881,51.6993834446145,24.2));
#27273=CARTESIAN_POINT('',(12.4038298031382,51.5921298605044,11.5));
#27274=CARTESIAN_POINT('',(12.4038298031382,51.5921298605044,14.5));
#27275=CARTESIAN_POINT('Ctrl Pts',(12.4038298031382,51.5921298605044,11.5));
#27276=CARTESIAN_POINT('Ctrl Pts',(12.2576427438577,51.7320306485686,11.4654707447276));
#27277=CARTESIAN_POINT('Ctrl Pts',(12.0690613826432,51.9125027175599,11.2969997378715));
#27278=CARTESIAN_POINT('Origin',(12.9670136041422,52.0078509283934,11.25));
#27279=CARTESIAN_POINT('',(13.2691061661509,51.3763922330071,11.5));
#27280=CARTESIAN_POINT('Origin',(12.9670136041422,52.0078509283934,11.5));
#27281=CARTESIAN_POINT('',(13.7150950830682,51.5021004224204,11.2969997378715));
#27282=CARTESIAN_POINT('Ctrl Pts',(13.7150950830682,51.5021004224204,11.2969997378715));
#27283=CARTESIAN_POINT('Ctrl Pts',(13.4638611198573,51.4312866298879,11.4654707447276));
#27284=CARTESIAN_POINT('Ctrl Pts',(13.2691061661509,51.3763922330071,11.5));
#27285=CARTESIAN_POINT('Ctrl Pts',(13.7150950830682,51.5021004224204,11.2969997378715));
#27286=CARTESIAN_POINT('Ctrl Pts',(13.7573545636769,51.3891532110793,11.1987310576087));
#27287=CARTESIAN_POINT('Ctrl Pts',(13.7926372892511,51.2745416453855,11.0971961933879));
#27288=CARTESIAN_POINT('Ctrl Pts',(13.8220767461304,51.1659085175284,11.));
#27289=CARTESIAN_POINT('Ctrl Pts',(12.0690613826432,51.9125027175599,11.2969997378715));
#27290=CARTESIAN_POINT('Ctrl Pts',(11.9787229721437,51.8326158735901,11.1987310576087));
#27291=CARTESIAN_POINT('Ctrl Pts',(11.8937633036688,51.7479841038615,11.0971961933879));
#27292=CARTESIAN_POINT('Ctrl Pts',(11.8167696417768,51.6658877329441,11.));
#27293=CARTESIAN_POINT('Origin',(12.9670136041422,52.0078509283934,11.));
#27294=CARTESIAN_POINT('',(13.2691061661509,51.3763922330071,24.2));
#27295=CARTESIAN_POINT('Origin',(12.9670136041422,52.0078509283934,24.2));
#27296=CARTESIAN_POINT('',(13.2691061661509,51.3763922330071,14.5));
#27297=CARTESIAN_POINT('Origin',(13.6826930157771,51.4929674483533,14.5));
#27298=CARTESIAN_POINT('',(14.0962798654034,51.6095426636995,24.2));
#27299=CARTESIAN_POINT('',(13.4184131650408,51.4184764906763,24.2));
#27300=CARTESIAN_POINT('',(14.0962798654034,51.6095426636995,11.5));
#27301=CARTESIAN_POINT('',(14.0962798654034,51.6095426636995,14.5));
#27302=CARTESIAN_POINT('Ctrl Pts',(14.0962798654034,51.6095426636995,11.5));
#27303=CARTESIAN_POINT('Ctrl Pts',(13.9053251952812,51.5557194296896,11.3977655520826));
#27304=CARTESIAN_POINT('Ctrl Pts',(13.7150950830682,51.5021004224204,11.2969997378715));
#27305=CARTESIAN_POINT('Origin',(15.683533661093,50.9192356256704,14.5));
#27306=CARTESIAN_POINT('',(15.6608948885132,50.9441513065986,11.2969997378715));
#27307=CARTESIAN_POINT('',(15.3945675730161,51.2372646541542,11.5));
#27308=CARTESIAN_POINT('Ctrl Pts',(15.6608948885132,50.9441513065986,11.2969997378715));
#27309=CARTESIAN_POINT('Ctrl Pts',(15.5279843488991,51.0904294047314,11.3977655520835));
#27310=CARTESIAN_POINT('Ctrl Pts',(15.3945675730161,51.2372646541542,11.5));
#27311=CARTESIAN_POINT('',(15.3945675730161,51.2372646541542,24.2));
#27312=CARTESIAN_POINT('',(15.3945675730161,51.2372646541542,14.5));
#27313=CARTESIAN_POINT('',(15.9724997491698,50.6012065971865,24.2));
#27314=CARTESIAN_POINT('',(15.8681814918784,50.7160167267776,24.2));
#27315=CARTESIAN_POINT('',(15.9724997491698,50.6012065971865,11.5));
#27316=CARTESIAN_POINT('',(15.9724997491698,50.6012065971865,14.5));
#27317=CARTESIAN_POINT('Ctrl Pts',(15.9724997491698,50.6012065971865,11.5));
#27318=CARTESIAN_POINT('Ctrl Pts',(15.8364277798677,50.7509640877247,11.4654707447276));
#27319=CARTESIAN_POINT('Ctrl Pts',(15.6608948885132,50.9441513065986,11.2969997378715));
#27320=CARTESIAN_POINT('Origin',(16.5633108984972,50.9766292734202,11.25));
#27321=CARTESIAN_POINT('',(16.8206192463028,50.3256358678088,11.5));
#27322=CARTESIAN_POINT('Origin',(16.5633108984972,50.9766292734202,11.5));
#27323=CARTESIAN_POINT('',(17.274290716648,50.4199272242176,11.2969997378715));
#27324=CARTESIAN_POINT('Ctrl Pts',(17.274290716648,50.4199272242176,11.2969997378715));
#27325=CARTESIAN_POINT('Ctrl Pts',(17.018729026285,50.366811125883,11.4654707447276));
#27326=CARTESIAN_POINT('Ctrl Pts',(16.8206192463028,50.3256358678088,11.5));
#27327=CARTESIAN_POINT('Ctrl Pts',(17.274290716648,50.4199272242176,11.2969997378715));
#27328=CARTESIAN_POINT('Ctrl Pts',(17.3085684561035,50.3043072742572,11.1987310576086));
#27329=CARTESIAN_POINT('Ctrl Pts',(17.3357703360584,50.1875136980568,11.0971961933879));
#27330=CARTESIAN_POINT('Ctrl Pts',(17.3575602159692,50.0770916023385,11.));
#27331=CARTESIAN_POINT('Ctrl Pts',(15.6608948885132,50.9441513065986,11.2969997378715));
#27332=CARTESIAN_POINT('Ctrl Pts',(15.5652039133075,50.8707607519257,11.1987310576086));
#27333=CARTESIAN_POINT('Ctrl Pts',(15.474547588492,50.7922616278179,11.0971961933879));
#27334=CARTESIAN_POINT('Ctrl Pts',(15.3920147259482,50.7157360458881,11.));
#27335=CARTESIAN_POINT('Origin',(16.5633108984972,50.9766292734202,11.));
#27336=CARTESIAN_POINT('',(16.8206192463028,50.3256358678088,24.2));
#27337=CARTESIAN_POINT('Origin',(16.5633108984972,50.9766292734202,24.2));
#27338=CARTESIAN_POINT('',(16.8206192463028,50.3256358678088,14.5));
#27339=CARTESIAN_POINT('Origin',(17.2413304950988,50.4130767515726,14.5));
#27340=CARTESIAN_POINT('',(17.6620417438948,50.5005176353364,24.2));
#27341=CARTESIAN_POINT('',(16.9724981902626,50.3572024805936,24.2));
#27342=CARTESIAN_POINT('',(17.6620417438948,50.5005176353364,11.5));
#27343=CARTESIAN_POINT('',(17.6620417438948,50.5005176353364,14.5));
#27344=CARTESIAN_POINT('Ctrl Pts',(17.6620417438948,50.5005176353364,11.5));
#27345=CARTESIAN_POINT('Ctrl Pts',(17.4677977107416,50.4601458364521,11.3977655520826));
#27346=CARTESIAN_POINT('Ctrl Pts',(17.274290716648,50.4199272242176,11.2969997378715));
#27347=CARTESIAN_POINT('Origin',(19.1972756843392,49.7011709228329,14.5));
#27348=CARTESIAN_POINT('',(19.1764300887141,49.7276051113597,11.2969997378715));
#27349=CARTESIAN_POINT('',(18.9311980867048,50.0385825039234,11.5));
#27350=CARTESIAN_POINT('Ctrl Pts',(19.1764300887141,49.7276051113597,11.2969997378715));
#27351=CARTESIAN_POINT('Ctrl Pts',(19.0540471568071,49.8827982539631,11.3977655520827));
#27352=CARTESIAN_POINT('Ctrl Pts',(18.9311980867048,50.0385825039234,11.5));
#27353=CARTESIAN_POINT('',(18.9311980867048,50.0385825039234,24.2));
#27354=CARTESIAN_POINT('',(18.9311980867048,50.0385825039234,14.5));
#27355=CARTESIAN_POINT('',(19.4633532819736,49.3637593417425,24.2));
#27356=CARTESIAN_POINT('',(19.3672978885042,49.485566673404,24.2));
#27357=CARTESIAN_POINT('',(19.4633532819736,49.3637593417425,11.5));
#27358=CARTESIAN_POINT('',(19.4633532819736,49.3637593417425,14.5));
#27359=CARTESIAN_POINT('Ctrl Pts',(19.4633532819736,49.3637593417425,11.5));
#27360=CARTESIAN_POINT('Ctrl Pts',(19.3380593316065,49.5226439313145,11.4654707447276));
#27361=CARTESIAN_POINT('Ctrl Pts',(19.1764300887141,49.7276051113597,11.2969997378715));
#27362=CARTESIAN_POINT('Origin',(20.0789134070929,49.6970546047798,11.25));
#27363=CARTESIAN_POINT('',(20.2901839602894,49.0296980633778,11.5));
#27364=CARTESIAN_POINT('Origin',(20.0789134070929,49.6970546047798,11.5));
#27365=CARTESIAN_POINT('',(20.7493277422619,49.0921132087718,11.2969997378715));
#27366=CARTESIAN_POINT('Ctrl Pts',(20.7493277422619,49.0921132087718,11.2969997378715));
#27367=CARTESIAN_POINT('Ctrl Pts',(20.4906833956133,49.056953580927,11.4654707447276));
#27368=CARTESIAN_POINT('Ctrl Pts',(20.2901839602894,49.0296980633778,11.5));
#27369=CARTESIAN_POINT('Ctrl Pts',(20.7493277422619,49.0921132087718,11.2969997378715));
#27370=CARTESIAN_POINT('Ctrl Pts',(20.7754567428632,48.9743838089661,11.1987310576086));
#27371=CARTESIAN_POINT('Ctrl Pts',(20.7944452523739,48.8559772288225,11.0971961933879));
#27372=CARTESIAN_POINT('Ctrl Pts',(20.8084793972118,48.7443041305937,11.));
#27373=CARTESIAN_POINT('Ctrl Pts',(19.1764300887141,49.7276051113597,11.2969997378715));
#27374=CARTESIAN_POINT('Ctrl Pts',(19.0758527456144,49.6610683973889,11.1987310576086));
#27375=CARTESIAN_POINT('Ctrl Pts',(18.9799414329601,49.5890843587438,11.0971961933879));
#27376=CARTESIAN_POINT('Ctrl Pts',(18.8922714615747,49.5185023907445,11.));
#27377=CARTESIAN_POINT('Origin',(20.0789134070929,49.6970546047798,11.));
#27378=CARTESIAN_POINT('',(20.2901839602894,49.0296980633778,24.2));
#27379=CARTESIAN_POINT('Origin',(20.0789134070929,49.6970546047798,24.2));
#27380=CARTESIAN_POINT('',(20.2901839602894,49.0296980633778,14.5));
#27381=CARTESIAN_POINT('Origin',(20.7159699453406,49.087578612363,14.5));
#27382=CARTESIAN_POINT('',(21.1417559303918,49.1454591613482,24.2));
#27383=CARTESIAN_POINT('',(20.4438949103711,49.0505932419138,24.2));
#27384=CARTESIAN_POINT('',(21.1417559303918,49.1454591613482,11.5));
#27385=CARTESIAN_POINT('',(21.1417559303918,49.1454591613482,14.5));
#27386=CARTESIAN_POINT('Ctrl Pts',(21.1417559303918,49.1454591613482,11.5));
#27387=CARTESIAN_POINT('Ctrl Pts',(20.9451688716126,49.1187354849356,11.397765552083));
#27388=CARTESIAN_POINT('Ctrl Pts',(20.7493277422619,49.0921132087718,11.2969997378715));
#27389=CARTESIAN_POINT('Origin',(22.6174905101547,48.2409671112037,14.5));
#27390=CARTESIAN_POINT('',(22.5985396491308,48.2687910226197,11.2969997378715));
#27391=CARTESIAN_POINT('',(22.3755977062724,48.5961174095941,11.5));
#27392=CARTESIAN_POINT('Ctrl Pts',(22.5985396491308,48.2687910226197,11.2969997378715));
#27393=CARTESIAN_POINT('Ctrl Pts',(22.4872805622718,48.4321431243046,11.3977655520831));
#27394=CARTESIAN_POINT('Ctrl Pts',(22.3755977062724,48.5961174095941,11.5));
#27395=CARTESIAN_POINT('',(22.3755977062724,48.5961174095941,24.2));
#27396=CARTESIAN_POINT('',(22.3755977062724,48.5961174095941,14.5));
#27397=CARTESIAN_POINT('',(22.859383314037,47.8858168128132,24.2));
#27398=CARTESIAN_POINT('',(22.7720587566113,48.0140279134694,24.2));
#27399=CARTESIAN_POINT('',(22.859383314037,47.8858168128132,11.5));
#27400=CARTESIAN_POINT('',(22.859383314037,47.8858168128132,14.5));
#27401=CARTESIAN_POINT('Ctrl Pts',(22.859383314037,47.8858168128132,11.5));
#27402=CARTESIAN_POINT('Ctrl Pts',(22.7454778021365,48.0530544316696,11.4654707447276));
#27403=CARTESIAN_POINT('Ctrl Pts',(22.5985396491308,48.2687910226197,11.2969997378715));
#27404=CARTESIAN_POINT('Origin',(23.4966934678946,48.1753608816354,11.25));
#27405=CARTESIAN_POINT('',(23.6608969375836,47.49489249843,11.5));
#27406=CARTESIAN_POINT('Origin',(23.4966934678946,48.1753608816354,11.5));
#27407=CARTESIAN_POINT('',(24.1232761288306,47.525127352495,11.2969997378715));
#27408=CARTESIAN_POINT('Ctrl Pts',(24.1232761288306,47.525127352495,11.2969997378715));
#27409=CARTESIAN_POINT('Ctrl Pts',(23.8628092151544,47.5080954893125,11.4654707447277));
#27410=CARTESIAN_POINT('Ctrl Pts',(23.6608969375836,47.49489249843,11.5));
#27411=CARTESIAN_POINT('Ctrl Pts',(24.1232761288306,47.525127352495,11.2969997378715));
#27412=CARTESIAN_POINT('Ctrl Pts',(24.1411290927132,47.4058620686457,11.1987310576087));
#27413=CARTESIAN_POINT('Ctrl Pts',(24.1518117216703,47.2864193495151,11.0971961933879));
#27414=CARTESIAN_POINT('Ctrl Pts',(24.1580217584921,47.174039308885,11.));
#27415=CARTESIAN_POINT('Ctrl Pts',(22.5985396491308,48.2687910226197,11.2969997378715));
#27416=CARTESIAN_POINT('Ctrl Pts',(22.4935659408428,48.2094323095332,11.1987310576086));
#27417=CARTESIAN_POINT('Ctrl Pts',(22.3928669106239,48.1443140553513,11.0971961933879));
#27418=CARTESIAN_POINT('Ctrl Pts',(22.300486949685,48.0800195695356,11.));
#27419=CARTESIAN_POINT('Origin',(23.4966934678946,48.1753608816354,11.));
#27420=CARTESIAN_POINT('',(23.6608969375836,47.49489249843,24.2));
#27421=CARTESIAN_POINT('Origin',(23.4966934678946,48.1753608816354,24.2));
#27422=CARTESIAN_POINT('',(23.6608969375836,47.49489249843,14.5));
#27423=CARTESIAN_POINT('Origin',(24.0896832723706,47.5229307244202,14.5));
#27424=CARTESIAN_POINT('',(24.5184696071576,47.5509689504103,24.2));
#27425=CARTESIAN_POINT('',(23.8156910294893,47.5050144435077,24.2));
#27426=CARTESIAN_POINT('',(24.5184696071576,47.5509689504103,11.5));
#27427=CARTESIAN_POINT('',(24.5184696071576,47.5509689504103,14.5));
#27428=CARTESIAN_POINT('Ctrl Pts',(24.5184696071576,47.5509689504103,11.5));
#27429=CARTESIAN_POINT('Ctrl Pts',(24.3204972751397,47.5380235915344,11.3977655520822));
#27430=CARTESIAN_POINT('Ctrl Pts',(24.1232761288306,47.525127352495,11.2969997378715));
#27431=CARTESIAN_POINT('Origin',(25.9275151957071,46.5457381569736,14.5));
#27432=CARTESIAN_POINT('',(25.9105513959743,46.5748162359794,11.2969997378715));
#27433=CARTESIAN_POINT('',(25.7109856630026,46.9168969161098,11.5));
#27434=CARTESIAN_POINT('Ctrl Pts',(25.9105513959743,46.5748162359794,11.2969997378715));
#27435=CARTESIAN_POINT('Ctrl Pts',(25.8109581972508,46.7455314617268,11.3977655520837));
#27436=CARTESIAN_POINT('Ctrl Pts',(25.7109856630026,46.9168969161098,11.5));
#27437=CARTESIAN_POINT('',(25.7109856630026,46.9168969161098,24.2));
#27438=CARTESIAN_POINT('',(25.7109856630026,46.9168969161098,14.5));
#27439=CARTESIAN_POINT('',(26.1440447284116,46.1745793978374,24.2));
#27440=CARTESIAN_POINT('',(26.0658764434955,46.3085696358935,24.2));
#27441=CARTESIAN_POINT('',(26.1440447284116,46.1745793978374,11.5));
#27442=CARTESIAN_POINT('',(26.1440447284116,46.1745793978374,14.5));
#27443=CARTESIAN_POINT('Ctrl Pts',(26.1440447284116,46.1745793978374,11.5));
#27444=CARTESIAN_POINT('Ctrl Pts',(26.0420825911821,46.3493552811098,11.4654707447276));
#27445=CARTESIAN_POINT('Ctrl Pts',(25.9105513959743,46.5748162359794,11.2969997378715));
#27446=CARTESIAN_POINT('Origin',(26.8,46.4189616428459,11.25));
#27447=CARTESIAN_POINT('',(26.9163364033829,45.7286965913998,11.5));
#27448=CARTESIAN_POINT('Origin',(26.8,46.4189616428459,11.5));
#27449=CARTESIAN_POINT('',(27.379698338963,45.7266038529658,11.2969997378715));
#27450=CARTESIAN_POINT('Ctrl Pts',(27.379698338963,45.7266038529658,11.2969997378715));
#27451=CARTESIAN_POINT('Ctrl Pts',(27.1186778268805,45.7277827319711,11.4654707447276));
#27452=CARTESIAN_POINT('Ctrl Pts',(26.9163364033829,45.7286965913998,11.5));
#27453=CARTESIAN_POINT('Ctrl Pts',(27.379698338963,45.7266038529658,11.2969997378715));
#27454=CARTESIAN_POINT('Ctrl Pts',(27.3891882882814,45.6063837335474,11.1987310576087));
#27455=CARTESIAN_POINT('Ctrl Pts',(27.3915129919902,45.4864867883511,11.0971961933879));
#27456=CARTESIAN_POINT('Ctrl Pts',(27.3898686661209,45.3739473095812,11.));
#27457=CARTESIAN_POINT('Ctrl Pts',(25.9105513959743,46.5748162359794,11.2969997378715));
#27458=CARTESIAN_POINT('Ctrl Pts',(25.8016927438527,46.5229247134606,11.1987310576086));
#27459=CARTESIAN_POINT('Ctrl Pts',(25.6966965916221,46.4649894933305,11.0971961933879));
#27460=CARTESIAN_POINT('Ctrl Pts',(25.6000567070134,46.4072957259707,11.));
#27461=CARTESIAN_POINT('Origin',(26.8,46.4189616428459,11.));
#27462=CARTESIAN_POINT('',(26.9163364033829,45.7286965913998,24.2));
#27463=CARTESIAN_POINT('Origin',(26.8,46.4189616428459,24.2));
#27464=CARTESIAN_POINT('',(26.9163364033829,45.7286965913998,14.5));
#27465=CARTESIAN_POINT('Origin',(27.3460340839842,45.7267558949762,14.5));
#27466=CARTESIAN_POINT('',(27.7757317645856,45.7248151985527,24.2));
#27467=CARTESIAN_POINT('',(27.0714594958567,45.7279959899203,24.2));
#27468=CARTESIAN_POINT('',(27.7757317645856,45.7248151985527,11.5));
#27469=CARTESIAN_POINT('',(27.7757317645856,45.7248151985527,14.5));
#27470=CARTESIAN_POINT('Ctrl Pts',(27.7757317645856,45.7248151985527,11.5));
#27471=CARTESIAN_POINT('Ctrl Pts',(27.5773386606331,45.7257112257008,11.3977655520829));
#27472=CARTESIAN_POINT('Ctrl Pts',(27.379698338963,45.7266038529658,11.2969997378715));
#27473=CARTESIAN_POINT('Origin',(29.1112236334504,44.6237430452042,14.5));
#27474=CARTESIAN_POINT('',(29.0963295409359,44.6539336263215,11.2969997378715));
#27475=CARTESIAN_POINT('',(28.9211122820413,45.0091020169205,11.5));
#27476=CARTESIAN_POINT('Ctrl Pts',(29.0963295409359,44.6539336263215,11.2969997378715));
#27477=CARTESIAN_POINT('Ctrl Pts',(29.0088874384024,44.8311802687091,11.3977655520826));
#27478=CARTESIAN_POINT('Ctrl Pts',(28.9211122820413,45.0091020169205,11.5));
#27479=CARTESIAN_POINT('',(28.9211122820413,45.0091020169205,24.2));
#27480=CARTESIAN_POINT('',(28.9211122820413,45.0091020169205,14.5));
#27481=CARTESIAN_POINT('',(29.3013349848595,44.2383840734879,24.2));
#27482=CARTESIAN_POINT('',(29.2327038004797,44.3775006619728,24.2));
#27483=CARTESIAN_POINT('',(29.3013349848595,44.2383840734879,11.5));
#27484=CARTESIAN_POINT('',(29.3013349848595,44.2383840734879,14.5));
#27485=CARTESIAN_POINT('Ctrl Pts',(29.3013349848595,44.2383840734879,11.5));
#27486=CARTESIAN_POINT('Ctrl Pts',(29.2118129715843,44.4198467306414,11.4654707447276));
#27487=CARTESIAN_POINT('Ctrl Pts',(29.0963295409359,44.6539336263215,11.2969997378715));
#27488=CARTESIAN_POINT('Origin',(29.972739626032,44.4364138889502,11.25));
#27489=CARTESIAN_POINT('',(30.0406421838457,43.7397150712088,11.5));
#27490=CARTESIAN_POINT('Origin',(29.972739626032,44.4364138889502,11.5));
#27491=CARTESIAN_POINT('',(30.5027294109855,43.705304935887,11.2969997378715));
#27492=CARTESIAN_POINT('Ctrl Pts',(30.5027294109855,43.705304935887,11.2969997378715));
#27493=CARTESIAN_POINT('Ctrl Pts',(30.242426966194,43.7246888137001,11.4654707447276));
#27494=CARTESIAN_POINT('Ctrl Pts',(30.0406421838457,43.7397150712088,11.5));
#27495=CARTESIAN_POINT('Ctrl Pts',(30.5027294109855,43.705304935887,11.2969997378715));
#27496=CARTESIAN_POINT('Ctrl Pts',(30.5038101116606,43.5847156812369,11.1987310576086));
#27497=CARTESIAN_POINT('Ctrl Pts',(30.4977655643985,43.4649486358398,11.0971961933879));
#27498=CARTESIAN_POINT('Ctrl Pts',(30.4882748868283,43.3527979999583,11.));
#27499=CARTESIAN_POINT('Ctrl Pts',(29.0963295409359,44.6539336263215,11.2969997378715));
#27500=CARTESIAN_POINT('Ctrl Pts',(28.9841162933916,44.609762104652,11.1987310576086));
#27501=CARTESIAN_POINT('Ctrl Pts',(28.8753345498489,44.5592921731428,11.0971961933878));
#27502=CARTESIAN_POINT('Ctrl Pts',(28.774905561374,44.5084802024738,11.));
#27503=CARTESIAN_POINT('Origin',(29.972739626032,44.4364138889502,11.));
#27504=CARTESIAN_POINT('',(30.0406421838457,43.7397150712088,24.2));
#27505=CARTESIAN_POINT('Origin',(29.972739626032,44.4364138889502,24.2));
#27506=CARTESIAN_POINT('',(30.0406421838457,43.7397150712088,14.5));
#27507=CARTESIAN_POINT('Origin',(32.1531051159017,42.4843455428814,14.5));
#27508=CARTESIAN_POINT('',(32.3158720826212,42.086663788759,11.0622545443403));
#27509=CARTESIAN_POINT('',(31.9903381491823,42.8820272970037,11.5));
#27510=CARTESIAN_POINT('Ctrl Pts',(32.3158720826212,42.086663788759,11.0622545443403));
#27511=CARTESIAN_POINT('Ctrl Pts',(32.153773743835,42.4827119120856,11.2776618075211));
#27512=CARTESIAN_POINT('Ctrl Pts',(31.9903381491823,42.8820272970037,11.5));
#27513=CARTESIAN_POINT('',(31.9903381491823,42.8820272970037,24.2));
#27514=CARTESIAN_POINT('',(31.9903381491823,42.8820272970037,14.5));
#27515=CARTESIAN_POINT('',(32.3158720826212,42.0866637887591,24.2));
#27516=CARTESIAN_POINT('',(32.2571123630091,42.2302289656376,24.2));
#27517=CARTESIAN_POINT('',(32.3158720826212,42.0866637887591,14.5));
#27518=CARTESIAN_POINT('Origin',(0.,0.,14.5));
#27519=CARTESIAN_POINT('',(30.8976733488635,43.6758947432898,11.5));
#27520=CARTESIAN_POINT('Origin',(0.,0.,11.5));
#27521=CARTESIAN_POINT('',(30.8976733488635,43.6758947432898,24.2));
#27522=CARTESIAN_POINT('',(30.8976733488635,43.6758947432898,14.5));
#27523=CARTESIAN_POINT('Origin',(0.,0.,24.2));
#27524=CARTESIAN_POINT('Origin',(0.,0.,11.25));
#27525=CARTESIAN_POINT('Ctrl Pts',(32.3467865928173,41.9843470488554,11.));
#27526=CARTESIAN_POINT('Ctrl Pts',(32.3333350107184,42.0190443039229,11.0192759649605));
#27527=CARTESIAN_POINT('Ctrl Pts',(32.3231696871195,42.0535642457408,11.0404458048696));
#27528=CARTESIAN_POINT('Ctrl Pts',(32.3158720826212,42.0866637887589,11.0622545443403));
#27529=CARTESIAN_POINT('Ctrl Pts',(30.8976733488635,43.6758947432898,11.5));
#27530=CARTESIAN_POINT('Ctrl Pts',(30.6998260242344,43.6906277911078,11.3977655520825));
#27531=CARTESIAN_POINT('Ctrl Pts',(30.5027294109855,43.705304935887,11.2969997378715));
#27532=CARTESIAN_POINT('Origin',(30.4691577663546,43.7078049072493,14.5));
#27533=CARTESIAN_POINT('',(30.195338532774,43.728195336432,24.2));
#27534=CARTESIAN_POINT('Origin',(-1.0407366972854,53.2696785416253,14.5));
#27535=CARTESIAN_POINT('',(-0.675303984907617,53.495737816465,24.2));
#27536=CARTESIAN_POINT('',(-1.40616940966319,53.0436192667856,24.2));
#27537=CARTESIAN_POINT('',(-1.27424630420037,53.1252278380639,24.2));
#27538=CARTESIAN_POINT('',(-0.675303984907617,53.495737816465,11.5));
#27539=CARTESIAN_POINT('',(-0.675303984907616,53.495737816465,14.5));
#27540=CARTESIAN_POINT('',(-1.4061694096633,53.0436192667855,11.0622545443403));
#27541=CARTESIAN_POINT('Ctrl Pts',(-0.675303984907617,53.495737816465,11.5));
#27542=CARTESIAN_POINT('Ctrl Pts',(-1.04223785273803,53.268749916186,11.2776618075198));
#27543=CARTESIAN_POINT('Ctrl Pts',(-1.4061694096633,53.0436192667855,11.0622545443403));
#27544=CARTESIAN_POINT('',(-1.40616940966319,53.0436192667856,14.5));
#27545=CARTESIAN_POINT('Origin',(0.,0.,11.25));
#27546=CARTESIAN_POINT('',(0.675303984907623,53.495737816465,11.5));
#27547=CARTESIAN_POINT('Origin',(0.,0.,11.5));
#27548=CARTESIAN_POINT('',(1.4061694096633,53.0436192667855,11.0622545443403));
#27549=CARTESIAN_POINT('Ctrl Pts',(1.4061694096633,53.0436192667855,11.0622545443403));
#27550=CARTESIAN_POINT('Ctrl Pts',(1.04223785273682,53.2687499161868,11.2776618075204));
#27551=CARTESIAN_POINT('Ctrl Pts',(0.675303984907623,53.495737816465,11.5));
#27552=CARTESIAN_POINT('Ctrl Pts',(1.49132004456262,52.9790143785696,11.));
#27553=CARTESIAN_POINT('Ctrl Pts',(1.46004295121972,52.9991784059996,11.0192759649605));
#27554=CARTESIAN_POINT('Ctrl Pts',(1.43152871896432,53.0211305982789,11.0404458048696));
#27555=CARTESIAN_POINT('Ctrl Pts',(1.40616940966333,53.0436192667855,11.0622545443404));
#27556=CARTESIAN_POINT('Ctrl Pts',(-1.40616940966334,53.0436192667855,11.0622545443403));
#27557=CARTESIAN_POINT('Ctrl Pts',(-1.43152871896432,53.0211305982789,11.0404458048696));
#27558=CARTESIAN_POINT('Ctrl Pts',(-1.46004295121971,52.9991784059996,11.0192759649605));
#27559=CARTESIAN_POINT('Ctrl Pts',(-1.49132004456262,52.9790143785696,11.));
#27560=CARTESIAN_POINT('Origin',(0.,0.,14.5));
#27561=CARTESIAN_POINT('',(0.675303984907623,53.495737816465,24.2));
#27562=CARTESIAN_POINT('Origin',(0.,0.,24.2));
#27563=CARTESIAN_POINT('',(0.675303984907623,53.495737816465,14.5));
#27564=CARTESIAN_POINT('Origin',(2.67770341754864,53.2125144041213,14.5));
#27565=CARTESIAN_POINT('',(2.29739178302177,53.0124970957196,11.0622545443404));
#27566=CARTESIAN_POINT('',(2.29739178302177,53.0124970957196,24.2));
#27567=CARTESIAN_POINT('',(2.29739178302177,53.0124970957196,14.5));
#27568=CARTESIAN_POINT('',(3.05801505207551,53.412531712523,24.2));
#27569=CARTESIAN_POINT('',(2.43468625658983,53.0847043819776,24.2));
#27570=CARTESIAN_POINT('',(3.05801505207551,53.412531712523,11.5));
#27571=CARTESIAN_POINT('',(3.0580150520755,53.412531712523,14.5));
#27572=CARTESIAN_POINT('Ctrl Pts',(3.05801505207551,53.412531712523,11.5));
#27573=CARTESIAN_POINT('Ctrl Pts',(2.8050919047221,53.2795118346824,11.352740724576));
#27574=CARTESIAN_POINT('Ctrl Pts',(2.55153997757952,53.14616126267,11.2067970124653));
#27575=CARTESIAN_POINT('Ctrl Pts',(2.29739178302176,53.0124970957196,11.0622545443404));
#27576=CARTESIAN_POINT('Origin',(0.,0.,11.25));
#27577=CARTESIAN_POINT('Ctrl Pts',(2.2079419616008,52.953989389792,11.));
#27578=CARTESIAN_POINT('Ctrl Pts',(2.24054908368457,52.9719223246298,11.0192757561174));
#27579=CARTESIAN_POINT('Ctrl Pts',(2.27052578922379,52.9918323934691,11.0404460254342));
#27580=CARTESIAN_POINT('Ctrl Pts',(2.29739178302177,53.0124970957196,11.0622545443404));
#27581=CARTESIAN_POINT('Origin',(0.,0.,11.5));
#27582=CARTESIAN_POINT('Origin',(0.,0.,11.25));
#27583=CARTESIAN_POINT('Origin',(0.,0.,11.5));
#27584=CARTESIAN_POINT('Origin',(0.,0.,11.25));
#27585=CARTESIAN_POINT('Origin',(0.,0.,11.5));
#27586=CARTESIAN_POINT('Origin',(0.,0.,11.25));
#27587=CARTESIAN_POINT('Origin',(0.,0.,11.5));
#27588=CARTESIAN_POINT('Origin',(0.,0.,11.25));
#27589=CARTESIAN_POINT('Origin',(0.,0.,11.5));
#27590=CARTESIAN_POINT('Origin',(0.,0.,11.25));
#27591=CARTESIAN_POINT('Origin',(0.,0.,11.5));
#27592=CARTESIAN_POINT('Origin',(0.,0.,11.25));
#27593=CARTESIAN_POINT('Origin',(0.,0.,11.5));
#27594=CARTESIAN_POINT('Origin',(0.,0.,11.25));
#27595=CARTESIAN_POINT('Origin',(0.,0.,11.5));
#27596=CARTESIAN_POINT('Origin',(0.,0.,14.5));
#27597=CARTESIAN_POINT('Origin',(0.,0.,24.2));
#27598=CARTESIAN_POINT('Origin',(0.,0.,14.5));
#27599=CARTESIAN_POINT('Origin',(0.,0.,24.2));
#27600=CARTESIAN_POINT('Origin',(0.,0.,14.5));
#27601=CARTESIAN_POINT('Origin',(0.,0.,24.2));
#27602=CARTESIAN_POINT('Origin',(0.,0.,14.5));
#27603=CARTESIAN_POINT('Origin',(0.,0.,24.2));
#27604=CARTESIAN_POINT('Origin',(0.,0.,14.5));
#27605=CARTESIAN_POINT('Origin',(0.,0.,24.2));
#27606=CARTESIAN_POINT('Origin',(0.,0.,14.5));
#27607=CARTESIAN_POINT('Origin',(0.,0.,24.2));
#27608=CARTESIAN_POINT('Origin',(0.,0.,14.5));
#27609=CARTESIAN_POINT('Origin',(0.,0.,24.2));
#27610=CARTESIAN_POINT('Origin',(0.,0.,14.5));
#27611=CARTESIAN_POINT('Origin',(0.,0.,24.2));
#27612=CARTESIAN_POINT('Origin',(1.04073669728541,53.2696785416253,14.5));
#27613=CARTESIAN_POINT('',(1.40616940966319,53.0436192667856,24.2));
#27614=CARTESIAN_POINT('',(1.27424630420038,53.1252278380639,24.2));
#27615=CARTESIAN_POINT('',(1.40616940966319,53.0436192667856,14.5));
#27616=CARTESIAN_POINT('Origin',(1.87061302325406,53.5673483282235,11.));
#27617=CARTESIAN_POINT('Origin',(1.87061302325406,53.5673483282235,24.2));
#27618=CARTESIAN_POINT('Origin',(-35.0383399022473,40.137968579585,14.5));
#27619=CARTESIAN_POINT('',(-34.9037103045182,40.546035650582,24.2));
#27620=CARTESIAN_POINT('',(-35.1729694999764,39.729901508588,24.2));
#27621=CARTESIAN_POINT('',(-35.1243675165795,39.8772158387497,24.2));
#27622=CARTESIAN_POINT('',(-34.9037103045182,40.546035650582,11.5));
#27623=CARTESIAN_POINT('',(-34.9037103045182,40.546035650582,14.5));
#27624=CARTESIAN_POINT('Ctrl Pts',(-34.9037103045182,40.546035650582,11.5));
#27625=CARTESIAN_POINT('Ctrl Pts',(-34.965869317664,40.3576294838967,11.397765552083));
#27626=CARTESIAN_POINT('Ctrl Pts',(-35.027792474811,40.1699382050837,11.2969997378714));
#27627=CARTESIAN_POINT('',(-35.1729694999764,39.729901508588,14.5));
#27628=CARTESIAN_POINT('Origin',(0.,0.,11.25));
#27629=CARTESIAN_POINT('',(-33.8690845744085,41.4141897191236,11.5));
#27630=CARTESIAN_POINT('Origin',(0.,0.,11.5));
#27631=CARTESIAN_POINT('',(-33.4771542514414,41.4710781664026,11.2969997378715));
#27632=CARTESIAN_POINT('Ctrl Pts',(-33.4771542514414,41.4710781664027,11.2969997378715));
#27633=CARTESIAN_POINT('Ctrl Pts',(-33.6727469213818,41.4426880096834,11.3977655520824));
#27634=CARTESIAN_POINT('Ctrl Pts',(-33.8690845744085,41.4141897191236,11.5));
#27635=CARTESIAN_POINT('Ctrl Pts',(-33.4771542514414,41.4710781664027,11.2969997378715));
#27636=CARTESIAN_POINT('Ctrl Pts',(-33.4698204384081,41.3507072752477,11.1987310576087));
#27637=CARTESIAN_POINT('Ctrl Pts',(-33.4554360886017,41.2316536226562,11.0971961933879));
#27638=CARTESIAN_POINT('Ctrl Pts',(-33.4381452969578,41.1204382162877,11.));
#27639=CARTESIAN_POINT('Origin',(0.,0.,14.5));
#27640=CARTESIAN_POINT('',(-33.8690845744085,41.4141897191236,24.2));
#27641=CARTESIAN_POINT('Origin',(0.,0.,24.2));
#27642=CARTESIAN_POINT('',(-33.8690845744085,41.4141897191236,14.5));
#27643=CARTESIAN_POINT('Origin',(-33.443838774836,41.4759138875076,14.5));
#27644=CARTESIAN_POINT('',(-33.0185929752635,41.5376380558916,24.2));
#27645=CARTESIAN_POINT('',(-33.1721089155843,41.5153553108074,24.2));
#27646=CARTESIAN_POINT('',(-33.0185929752635,41.5376380558916,11.5));
#27647=CARTESIAN_POINT('',(-33.0185929752635,41.5376380558916,14.5));
#27648=CARTESIAN_POINT('Ctrl Pts',(-33.0185929752635,41.5376380558916,11.5));
#27649=CARTESIAN_POINT('Ctrl Pts',(-33.2188380412863,41.5085726067192,11.4654707447276));
#27650=CARTESIAN_POINT('Ctrl Pts',(-33.4771542514414,41.4710781664026,11.2969997378715));
#27651=CARTESIAN_POINT('Origin',(-32.1531051159017,42.4843455428814,14.5));
#27652=CARTESIAN_POINT('',(-31.9903381491823,42.8820272970037,24.2));
#27653=CARTESIAN_POINT('',(-32.3158720826212,42.0866637887591,24.2));
#27654=CARTESIAN_POINT('',(-32.2571123630091,42.2302289656376,24.2));
#27655=CARTESIAN_POINT('',(-31.9903381491823,42.8820272970037,11.5));
#27656=CARTESIAN_POINT('',(-31.9903381491823,42.8820272970037,14.5));
#27657=CARTESIAN_POINT('',(-32.140353293127,42.5155015406339,11.2969997378715));
#27658=CARTESIAN_POINT('Ctrl Pts',(-31.9903381491823,42.8820272970037,11.5));
#27659=CARTESIAN_POINT('Ctrl Pts',(-32.0654882959164,42.6984160718386,11.3977655520826));
#27660=CARTESIAN_POINT('Ctrl Pts',(-32.140353293127,42.5155015406339,11.2969997378715));
#27661=CARTESIAN_POINT('',(-32.3158720826212,42.0866637887591,11.5));
#27662=CARTESIAN_POINT('Ctrl Pts',(-32.140353293127,42.5155015406339,11.2969997378715));
#27663=CARTESIAN_POINT('Ctrl Pts',(-32.2392263355501,42.2739291519686,11.4654707447276));
#27664=CARTESIAN_POINT('Ctrl Pts',(-32.3158720826212,42.0866637887591,11.5));
#27665=CARTESIAN_POINT('',(-32.3158720826212,42.0866637887591,14.5));
#27666=CARTESIAN_POINT('Origin',(0.,0.,11.25));
#27667=CARTESIAN_POINT('',(-30.8976733488635,43.6758947432898,11.5));
#27668=CARTESIAN_POINT('Origin',(0.,0.,11.5));
#27669=CARTESIAN_POINT('',(-30.5027294109855,43.705304935887,11.2969997378715));
#27670=CARTESIAN_POINT('Ctrl Pts',(-30.5027294109855,43.705304935887,11.2969997378715));
#27671=CARTESIAN_POINT('Ctrl Pts',(-30.699826024235,43.6906277911078,11.3977655520827));
#27672=CARTESIAN_POINT('Ctrl Pts',(-30.8976733488635,43.6758947432898,11.5));
#27673=CARTESIAN_POINT('Ctrl Pts',(-30.5027294109855,43.705304935887,11.2969997378715));
#27674=CARTESIAN_POINT('Ctrl Pts',(-30.5038101116606,43.5847156812369,11.1987310576086));
#27675=CARTESIAN_POINT('Ctrl Pts',(-30.4977655643985,43.4649486358399,11.0971961933879));
#27676=CARTESIAN_POINT('Ctrl Pts',(-30.4882748868283,43.3527979999583,11.));
#27677=CARTESIAN_POINT('Ctrl Pts',(-32.140353293127,42.5155015406339,11.2969997378715));
#27678=CARTESIAN_POINT('Ctrl Pts',(-32.0253321418224,42.4792652190273,11.1987310576087));
#27679=CARTESIAN_POINT('Ctrl Pts',(-31.9132947806875,42.4365064605718,11.0971961933879));
#27680=CARTESIAN_POINT('Ctrl Pts',(-31.809565968283,42.3928238374073,11.));
#27681=CARTESIAN_POINT('Origin',(0.,0.,14.5));
#27682=CARTESIAN_POINT('',(-30.8976733488635,43.6758947432898,24.2));
#27683=CARTESIAN_POINT('Origin',(0.,0.,24.2));
#27684=CARTESIAN_POINT('',(-30.8976733488635,43.6758947432898,14.5));
#27685=CARTESIAN_POINT('Origin',(-30.4691577663546,43.7078049072493,14.5));
#27686=CARTESIAN_POINT('',(-30.0406421838457,43.7397150712088,24.2));
#27687=CARTESIAN_POINT('',(-30.195338532774,43.728195336432,24.2));
#27688=CARTESIAN_POINT('',(-30.0406421838457,43.7397150712088,11.5));
#27689=CARTESIAN_POINT('',(-30.0406421838457,43.7397150712088,14.5));
#27690=CARTESIAN_POINT('Ctrl Pts',(-30.0406421838457,43.7397150712088,11.5));
#27691=CARTESIAN_POINT('Ctrl Pts',(-30.242426966194,43.7246888137001,11.4654707447276));
#27692=CARTESIAN_POINT('Ctrl Pts',(-30.5027294109855,43.705304935887,11.2969997378715));
#27693=CARTESIAN_POINT('Origin',(-29.1112236334504,44.6237430452042,14.5));
#27694=CARTESIAN_POINT('',(-28.9211122820413,45.0091020169205,24.2));
#27695=CARTESIAN_POINT('',(-29.3013349848595,44.2383840734879,24.2));
#27696=CARTESIAN_POINT('',(-29.2327038004797,44.3775006619728,24.2));
#27697=CARTESIAN_POINT('',(-28.9211122820413,45.0091020169205,11.5));
#27698=CARTESIAN_POINT('',(-28.9211122820413,45.0091020169205,14.5));
#27699=CARTESIAN_POINT('',(-29.0963295409359,44.6539336263215,11.2969997378715));
#27700=CARTESIAN_POINT('Ctrl Pts',(-28.9211122820413,45.0091020169205,11.5));
#27701=CARTESIAN_POINT('Ctrl Pts',(-29.0088874384022,44.8311802687095,11.3977655520828));
#27702=CARTESIAN_POINT('Ctrl Pts',(-29.0963295409359,44.6539336263215,11.2969997378715));
#27703=CARTESIAN_POINT('',(-29.3013349848595,44.2383840734879,11.5));
#27704=CARTESIAN_POINT('Ctrl Pts',(-29.0963295409359,44.6539336263215,11.2969997378715));
#27705=CARTESIAN_POINT('Ctrl Pts',(-29.2118129715843,44.4198467306414,11.4654707447276));
#27706=CARTESIAN_POINT('Ctrl Pts',(-29.3013349848595,44.2383840734879,11.5));
#27707=CARTESIAN_POINT('',(-29.3013349848595,44.2383840734879,14.5));
#27708=CARTESIAN_POINT('Origin',(0.,0.,11.25));
#27709=CARTESIAN_POINT('',(-27.7757317645856,45.7248151985527,11.5));
#27710=CARTESIAN_POINT('Origin',(0.,0.,11.5));
#27711=CARTESIAN_POINT('',(-27.3796983389629,45.7266038529658,11.2969997378715));
#27712=CARTESIAN_POINT('Ctrl Pts',(-27.3796983389629,45.7266038529658,11.2969997378715));
#27713=CARTESIAN_POINT('Ctrl Pts',(-27.5773386606337,45.7257112257008,11.3977655520832));
#27714=CARTESIAN_POINT('Ctrl Pts',(-27.7757317645856,45.7248151985527,11.5));
#27715=CARTESIAN_POINT('Ctrl Pts',(-27.3796983389629,45.7266038529658,11.2969997378715));
#27716=CARTESIAN_POINT('Ctrl Pts',(-27.3891882882814,45.6063837335474,11.1987310576087));
#27717=CARTESIAN_POINT('Ctrl Pts',(-27.3915129919902,45.4864867883511,11.0971961933879));
#27718=CARTESIAN_POINT('Ctrl Pts',(-27.3898686661209,45.3739473095812,11.));
#27719=CARTESIAN_POINT('Ctrl Pts',(-29.0963295409359,44.6539336263215,11.2969997378715));
#27720=CARTESIAN_POINT('Ctrl Pts',(-28.9841162933917,44.6097621046521,11.1987310576087));
#27721=CARTESIAN_POINT('Ctrl Pts',(-28.875334549849,44.5592921731428,11.0971961933879));
#27722=CARTESIAN_POINT('Ctrl Pts',(-28.774905561374,44.5084802024738,11.));
#27723=CARTESIAN_POINT('Origin',(0.,0.,14.5));
#27724=CARTESIAN_POINT('',(-27.7757317645856,45.7248151985527,24.2));
#27725=CARTESIAN_POINT('Origin',(0.,0.,24.2));
#27726=CARTESIAN_POINT('',(-27.7757317645856,45.7248151985527,14.5));
#27727=CARTESIAN_POINT('Origin',(-27.3460340839842,45.7267558949762,14.5));
#27728=CARTESIAN_POINT('',(-26.9163364033829,45.7286965913998,24.2));
#27729=CARTESIAN_POINT('',(-27.0714594958567,45.7279959899203,24.2));
#27730=CARTESIAN_POINT('',(-26.9163364033829,45.7286965913998,11.5));
#27731=CARTESIAN_POINT('',(-26.9163364033829,45.7286965913998,14.5));
#27732=CARTESIAN_POINT('Ctrl Pts',(-26.9163364033829,45.7286965913998,11.5));
#27733=CARTESIAN_POINT('Ctrl Pts',(-27.1186778268805,45.7277827319711,11.4654707447276));
#27734=CARTESIAN_POINT('Ctrl Pts',(-27.3796983389629,45.7266038529658,11.2969997378715));
#27735=CARTESIAN_POINT('Origin',(-25.927515195707,46.5457381569737,14.5));
#27736=CARTESIAN_POINT('',(-25.7109856630023,46.91689691611,24.2));
#27737=CARTESIAN_POINT('',(-26.1440447284116,46.1745793978375,24.2));
#27738=CARTESIAN_POINT('',(-26.0658764434955,46.3085696358935,24.2));
#27739=CARTESIAN_POINT('',(-25.7109856630023,46.91689691611,11.5));
#27740=CARTESIAN_POINT('',(-25.7109856630023,46.91689691611,14.5));
#27741=CARTESIAN_POINT('',(-25.9105513959742,46.5748162359794,11.2969997378715));
#27742=CARTESIAN_POINT('Ctrl Pts',(-25.7109856630023,46.91689691611,11.5));
#27743=CARTESIAN_POINT('Ctrl Pts',(-25.8109581972516,46.7455314617252,11.3977655520827));
#27744=CARTESIAN_POINT('Ctrl Pts',(-25.9105513959742,46.5748162359794,11.2969997378715));
#27745=CARTESIAN_POINT('',(-26.1440447284116,46.1745793978375,11.5));
#27746=CARTESIAN_POINT('Ctrl Pts',(-25.9105513959742,46.5748162359794,11.2969997378715));
#27747=CARTESIAN_POINT('Ctrl Pts',(-26.042082591182,46.3493552811099,11.4654707447276));
#27748=CARTESIAN_POINT('Ctrl Pts',(-26.1440447284116,46.1745793978375,11.5));
#27749=CARTESIAN_POINT('',(-26.1440447284116,46.1745793978375,14.5));
#27750=CARTESIAN_POINT('Origin',(0.,0.,11.25));
#27751=CARTESIAN_POINT('',(-24.5184696071579,47.5509689504102,11.5));
#27752=CARTESIAN_POINT('Origin',(0.,0.,11.5));
#27753=CARTESIAN_POINT('',(-24.1232761288307,47.5251273524949,11.2969997378715));
#27754=CARTESIAN_POINT('Ctrl Pts',(-24.1232761288307,47.5251273524949,11.2969997378715));
#27755=CARTESIAN_POINT('Ctrl Pts',(-24.3204972751416,47.5380235915344,11.3977655520831));
#27756=CARTESIAN_POINT('Ctrl Pts',(-24.5184696071579,47.5509689504102,11.5));
#27757=CARTESIAN_POINT('Ctrl Pts',(-24.1232761288307,47.5251273524949,11.2969997378715));
#27758=CARTESIAN_POINT('Ctrl Pts',(-24.1411290927132,47.4058620686457,11.1987310576086));
#27759=CARTESIAN_POINT('Ctrl Pts',(-24.1518117216703,47.2864193495151,11.0971961933879));
#27760=CARTESIAN_POINT('Ctrl Pts',(-24.1580217584921,47.174039308885,11.));
#27761=CARTESIAN_POINT('Ctrl Pts',(-25.9105513959742,46.5748162359794,11.2969997378715));
#27762=CARTESIAN_POINT('Ctrl Pts',(-25.8016927438527,46.5229247134606,11.1987310576086));
#27763=CARTESIAN_POINT('Ctrl Pts',(-25.6966965916221,46.4649894933305,11.0971961933879));
#27764=CARTESIAN_POINT('Ctrl Pts',(-25.6000567070134,46.4072957259707,11.));
#27765=CARTESIAN_POINT('Origin',(0.,0.,14.5));
#27766=CARTESIAN_POINT('',(-24.5184696071579,47.5509689504102,24.2));
#27767=CARTESIAN_POINT('Origin',(0.,0.,24.2));
#27768=CARTESIAN_POINT('',(-24.5184696071579,47.5509689504102,14.5));
#27769=CARTESIAN_POINT('Origin',(-24.0896832723708,47.5229307244201,14.5));
#27770=CARTESIAN_POINT('',(-23.6608969375837,47.49489249843,24.2));
#27771=CARTESIAN_POINT('',(-23.8156910294893,47.5050144435077,24.2));
#27772=CARTESIAN_POINT('',(-23.6608969375837,47.49489249843,11.5));
#27773=CARTESIAN_POINT('',(-23.6608969375837,47.49489249843,14.5));
#27774=CARTESIAN_POINT('Ctrl Pts',(-23.6608969375837,47.49489249843,11.5));
#27775=CARTESIAN_POINT('Ctrl Pts',(-23.8628092151544,47.5080954893125,11.4654707447276));
#27776=CARTESIAN_POINT('Ctrl Pts',(-24.1232761288307,47.5251273524949,11.2969997378715));
#27777=CARTESIAN_POINT('Origin',(-22.6174905101547,48.2409671112037,14.5));
#27778=CARTESIAN_POINT('',(-22.3755977062724,48.5961174095941,24.2));
#27779=CARTESIAN_POINT('',(-22.859383314037,47.8858168128132,24.2));
#27780=CARTESIAN_POINT('',(-22.7720587566113,48.0140279134694,24.2));
#27781=CARTESIAN_POINT('',(-22.3755977062724,48.5961174095941,11.5));
#27782=CARTESIAN_POINT('',(-22.3755977062724,48.5961174095941,14.5));
#27783=CARTESIAN_POINT('',(-22.5985396491308,48.2687910226197,11.2969997378715));
#27784=CARTESIAN_POINT('Ctrl Pts',(-22.3755977062724,48.5961174095941,11.5));
#27785=CARTESIAN_POINT('Ctrl Pts',(-22.4872805622725,48.4321431243035,11.3977655520824));
#27786=CARTESIAN_POINT('Ctrl Pts',(-22.5985396491308,48.2687910226197,11.2969997378715));
#27787=CARTESIAN_POINT('',(-22.859383314037,47.8858168128132,11.5));
#27788=CARTESIAN_POINT('Ctrl Pts',(-22.5985396491308,48.2687910226197,11.2969997378715));
#27789=CARTESIAN_POINT('Ctrl Pts',(-22.7454778021365,48.0530544316697,11.4654707447276));
#27790=CARTESIAN_POINT('Ctrl Pts',(-22.859383314037,47.8858168128132,11.5));
#27791=CARTESIAN_POINT('',(-22.859383314037,47.8858168128132,14.5));
#27792=CARTESIAN_POINT('Origin',(0.,0.,11.25));
#27793=CARTESIAN_POINT('',(-21.1417559303918,49.1454591613482,11.5));
#27794=CARTESIAN_POINT('Origin',(0.,0.,11.5));
#27795=CARTESIAN_POINT('',(-20.7493277422619,49.0921132087718,11.2969997378715));
#27796=CARTESIAN_POINT('Ctrl Pts',(-20.7493277422619,49.0921132087718,11.2969997378715));
#27797=CARTESIAN_POINT('Ctrl Pts',(-20.9451688716126,49.1187354849356,11.397765552083));
#27798=CARTESIAN_POINT('Ctrl Pts',(-21.1417559303918,49.1454591613482,11.5));
#27799=CARTESIAN_POINT('Ctrl Pts',(-20.7493277422619,49.0921132087718,11.2969997378715));
#27800=CARTESIAN_POINT('Ctrl Pts',(-20.7754567428632,48.9743838089661,11.1987310576086));
#27801=CARTESIAN_POINT('Ctrl Pts',(-20.7944452523739,48.8559772288225,11.0971961933878));
#27802=CARTESIAN_POINT('Ctrl Pts',(-20.8084793972118,48.7443041305937,11.));
#27803=CARTESIAN_POINT('Ctrl Pts',(-22.5985396491308,48.2687910226197,11.2969997378715));
#27804=CARTESIAN_POINT('Ctrl Pts',(-22.4935659408428,48.2094323095331,11.1987310576086));
#27805=CARTESIAN_POINT('Ctrl Pts',(-22.3928669106238,48.1443140553513,11.0971961933879));
#27806=CARTESIAN_POINT('Ctrl Pts',(-22.300486949685,48.0800195695356,11.));
#27807=CARTESIAN_POINT('Origin',(0.,0.,14.5));
#27808=CARTESIAN_POINT('',(-21.1417559303918,49.1454591613482,24.2));
#27809=CARTESIAN_POINT('Origin',(0.,0.,24.2));
#27810=CARTESIAN_POINT('',(-21.1417559303918,49.1454591613482,14.5));
#27811=CARTESIAN_POINT('Origin',(-20.7159699453406,49.087578612363,14.5));
#27812=CARTESIAN_POINT('',(-20.2901839602894,49.0296980633778,24.2));
#27813=CARTESIAN_POINT('',(-20.4438949103711,49.0505932419138,24.2));
#27814=CARTESIAN_POINT('',(-20.2901839602894,49.0296980633778,11.5));
#27815=CARTESIAN_POINT('',(-20.2901839602894,49.0296980633778,14.5));
#27816=CARTESIAN_POINT('Ctrl Pts',(-20.2901839602894,49.0296980633778,11.5));
#27817=CARTESIAN_POINT('Ctrl Pts',(-20.4906833956133,49.056953580927,11.4654707447276));
#27818=CARTESIAN_POINT('Ctrl Pts',(-20.7493277422619,49.0921132087718,11.2969997378715));
#27819=CARTESIAN_POINT('Origin',(-19.1972756843392,49.7011709228329,14.5));
#27820=CARTESIAN_POINT('',(-18.9311980867048,50.0385825039234,24.2));
#27821=CARTESIAN_POINT('',(-19.4633532819736,49.3637593417425,24.2));
#27822=CARTESIAN_POINT('',(-19.3672978885042,49.485566673404,24.2));
#27823=CARTESIAN_POINT('',(-18.9311980867048,50.0385825039234,11.5));
#27824=CARTESIAN_POINT('',(-18.9311980867048,50.0385825039234,14.5));
#27825=CARTESIAN_POINT('',(-19.1764300887141,49.7276051113597,11.2969997378715));
#27826=CARTESIAN_POINT('Ctrl Pts',(-18.9311980867048,50.0385825039234,11.5));
#27827=CARTESIAN_POINT('Ctrl Pts',(-19.0540471568067,49.8827982539635,11.397765552083));
#27828=CARTESIAN_POINT('Ctrl Pts',(-19.1764300887141,49.7276051113597,11.2969997378715));
#27829=CARTESIAN_POINT('',(-19.4633532819736,49.3637593417425,11.5));
#27830=CARTESIAN_POINT('Ctrl Pts',(-19.1764300887141,49.7276051113597,11.2969997378715));
#27831=CARTESIAN_POINT('Ctrl Pts',(-19.3380593316064,49.5226439313145,11.4654707447276));
#27832=CARTESIAN_POINT('Ctrl Pts',(-19.4633532819736,49.3637593417425,11.5));
#27833=CARTESIAN_POINT('',(-19.4633532819736,49.3637593417425,14.5));
#27834=CARTESIAN_POINT('Origin',(0.,0.,11.25));
#27835=CARTESIAN_POINT('',(-17.6620417438945,50.5005176353365,11.5));
#27836=CARTESIAN_POINT('Origin',(0.,0.,11.5));
#27837=CARTESIAN_POINT('',(-17.274290716648,50.4199272242177,11.2969997378715));
#27838=CARTESIAN_POINT('Ctrl Pts',(-17.274290716648,50.4199272242177,11.2969997378715));
#27839=CARTESIAN_POINT('Ctrl Pts',(-17.4677977107421,50.4601458364523,11.397765552083));
#27840=CARTESIAN_POINT('Ctrl Pts',(-17.6620417438945,50.5005176353365,11.5));
#27841=CARTESIAN_POINT('Ctrl Pts',(-17.274290716648,50.4199272242177,11.2969997378715));
#27842=CARTESIAN_POINT('Ctrl Pts',(-17.3085684561035,50.3043072742572,11.1987310576086));
#27843=CARTESIAN_POINT('Ctrl Pts',(-17.3357703360584,50.1875136980568,11.0971961933879));
#27844=CARTESIAN_POINT('Ctrl Pts',(-17.3575602159693,50.0770916023385,11.));
#27845=CARTESIAN_POINT('Ctrl Pts',(-19.1764300887141,49.7276051113597,11.2969997378715));
#27846=CARTESIAN_POINT('Ctrl Pts',(-19.0758527456144,49.6610683973889,11.1987310576086));
#27847=CARTESIAN_POINT('Ctrl Pts',(-18.9799414329601,49.5890843587438,11.0971961933879));
#27848=CARTESIAN_POINT('Ctrl Pts',(-18.8922714615747,49.5185023907445,11.));
#27849=CARTESIAN_POINT('Origin',(0.,0.,14.5));
#27850=CARTESIAN_POINT('',(-17.6620417438945,50.5005176353365,24.2));
#27851=CARTESIAN_POINT('Origin',(0.,0.,24.2));
#27852=CARTESIAN_POINT('',(-17.6620417438945,50.5005176353365,14.5));
#27853=CARTESIAN_POINT('Origin',(-17.2413304950986,50.4130767515726,14.5));
#27854=CARTESIAN_POINT('',(-16.8206192463027,50.3256358678088,24.2));
#27855=CARTESIAN_POINT('',(-16.9724981902626,50.3572024805937,24.2));
#27856=CARTESIAN_POINT('',(-16.8206192463027,50.3256358678088,11.5));
#27857=CARTESIAN_POINT('',(-16.8206192463027,50.3256358678088,14.5));
#27858=CARTESIAN_POINT('Ctrl Pts',(-16.8206192463027,50.3256358678088,11.5));
#27859=CARTESIAN_POINT('Ctrl Pts',(-17.0187290262849,50.366811125883,11.4654707447276));
#27860=CARTESIAN_POINT('Ctrl Pts',(-17.274290716648,50.4199272242177,11.2969997378715));
#27861=CARTESIAN_POINT('Origin',(-15.683533661093,50.9192356256704,14.5));
#27862=CARTESIAN_POINT('',(-15.3945675730161,51.2372646541542,24.2));
#27863=CARTESIAN_POINT('',(-15.9724997491698,50.6012065971865,24.2));
#27864=CARTESIAN_POINT('',(-15.8681814918784,50.7160167267776,24.2));
#27865=CARTESIAN_POINT('',(-15.3945675730161,51.2372646541542,11.5));
#27866=CARTESIAN_POINT('',(-15.3945675730161,51.2372646541542,14.5));
#27867=CARTESIAN_POINT('',(-15.6608948885132,50.9441513065986,11.2969997378715));
#27868=CARTESIAN_POINT('Ctrl Pts',(-15.3945675730161,51.2372646541542,11.5));
#27869=CARTESIAN_POINT('Ctrl Pts',(-15.5279843488997,51.0904294047306,11.397765552083));
#27870=CARTESIAN_POINT('Ctrl Pts',(-15.6608948885132,50.9441513065986,11.2969997378715));
#27871=CARTESIAN_POINT('',(-15.9724997491698,50.6012065971865,11.5));
#27872=CARTESIAN_POINT('Ctrl Pts',(-15.6608948885132,50.9441513065986,11.2969997378715));
#27873=CARTESIAN_POINT('Ctrl Pts',(-15.8364277798677,50.7509640877247,11.4654707447276));
#27874=CARTESIAN_POINT('Ctrl Pts',(-15.9724997491698,50.6012065971865,11.5));
#27875=CARTESIAN_POINT('',(-15.9724997491698,50.6012065971865,14.5));
#27876=CARTESIAN_POINT('Origin',(0.,0.,11.25));
#27877=CARTESIAN_POINT('',(-14.0962798654037,51.6095426636995,11.5));
#27878=CARTESIAN_POINT('Origin',(0.,0.,11.5));
#27879=CARTESIAN_POINT('',(-13.7150950830682,51.5021004224203,11.2969997378715));
#27880=CARTESIAN_POINT('Ctrl Pts',(-13.7150950830682,51.5021004224203,11.2969997378715));
#27881=CARTESIAN_POINT('Ctrl Pts',(-13.9053251952821,51.5557194296898,11.3977655520829));
#27882=CARTESIAN_POINT('Ctrl Pts',(-14.0962798654037,51.6095426636995,11.5));
#27883=CARTESIAN_POINT('Ctrl Pts',(-13.7150950830682,51.5021004224203,11.2969997378715));
#27884=CARTESIAN_POINT('Ctrl Pts',(-13.7573545636769,51.3891532110793,11.1987310576086));
#27885=CARTESIAN_POINT('Ctrl Pts',(-13.7926372892511,51.2745416453855,11.0971961933879));
#27886=CARTESIAN_POINT('Ctrl Pts',(-13.8220767461304,51.1659085175284,11.));
#27887=CARTESIAN_POINT('Ctrl Pts',(-15.6608948885132,50.9441513065986,11.2969997378715));
#27888=CARTESIAN_POINT('Ctrl Pts',(-15.5652039133075,50.8707607519257,11.1987310576086));
#27889=CARTESIAN_POINT('Ctrl Pts',(-15.474547588492,50.7922616278179,11.0971961933879));
#27890=CARTESIAN_POINT('Ctrl Pts',(-15.3920147259482,50.7157360458881,11.));
#27891=CARTESIAN_POINT('Origin',(0.,0.,14.5));
#27892=CARTESIAN_POINT('',(-14.0962798654037,51.6095426636995,24.2));
#27893=CARTESIAN_POINT('Origin',(0.,0.,24.2));
#27894=CARTESIAN_POINT('',(-14.0962798654037,51.6095426636995,14.5));
#27895=CARTESIAN_POINT('Origin',(-13.6826930157773,51.4929674483533,14.5));
#27896=CARTESIAN_POINT('',(-13.269106166151,51.3763922330071,24.2));
#27897=CARTESIAN_POINT('',(-13.4184131650408,51.4184764906763,24.2));
#27898=CARTESIAN_POINT('',(-13.269106166151,51.3763922330071,11.5));
#27899=CARTESIAN_POINT('',(-13.269106166151,51.3763922330071,14.5));
#27900=CARTESIAN_POINT('Ctrl Pts',(-13.269106166151,51.3763922330071,11.5));
#27901=CARTESIAN_POINT('Ctrl Pts',(-13.4638611198573,51.4312866298879,11.4654707447276));
#27902=CARTESIAN_POINT('Ctrl Pts',(-13.7150950830682,51.5021004224203,11.2969997378715));
#27903=CARTESIAN_POINT('Origin',(-12.0933830383532,51.8892269309232,14.5));
#27904=CARTESIAN_POINT('',(-11.7829362735682,52.1863240013419,24.2));
#27905=CARTESIAN_POINT('',(-12.4038298031382,51.5921298605045,24.2));
#27906=CARTESIAN_POINT('',(-12.2917569100881,51.6993834446145,24.2));
#27907=CARTESIAN_POINT('',(-11.7829362735682,52.1863240013419,11.5));
#27908=CARTESIAN_POINT('',(-11.7829362735682,52.1863240013419,14.5));
#27909=CARTESIAN_POINT('',(-12.0690613826432,51.9125027175599,11.2969997378715));
#27910=CARTESIAN_POINT('Ctrl Pts',(-11.7829362735682,52.1863240013419,11.5));
#27911=CARTESIAN_POINT('Ctrl Pts',(-11.9262707621139,52.0491531190285,11.397765552082));
#27912=CARTESIAN_POINT('Ctrl Pts',(-12.0690613826432,51.9125027175599,11.2969997378715));
#27913=CARTESIAN_POINT('',(-12.4038298031382,51.5921298605045,11.5));
#27914=CARTESIAN_POINT('Ctrl Pts',(-12.0690613826432,51.9125027175599,11.2969997378715));
#27915=CARTESIAN_POINT('Ctrl Pts',(-12.2576427438576,51.7320306485686,11.4654707447276));
#27916=CARTESIAN_POINT('Ctrl Pts',(-12.4038298031382,51.5921298605045,11.5));
#27917=CARTESIAN_POINT('',(-12.4038298031382,51.5921298605045,14.5));
#27918=CARTESIAN_POINT('Origin',(0.,0.,11.25));
#27919=CARTESIAN_POINT('',(-10.4618423283614,52.4671311879781,11.5));
#27920=CARTESIAN_POINT('Origin',(0.,0.,11.5));
#27921=CARTESIAN_POINT('',(-10.0890808848803,52.3333605643381,11.2969997378715));
#27922=CARTESIAN_POINT('Ctrl Pts',(-10.0890808848803,52.3333605643381,11.2969997378715));
#27923=CARTESIAN_POINT('Ctrl Pts',(-10.275107333228,52.4001187402283,11.3977655520824));
#27924=CARTESIAN_POINT('Ctrl Pts',(-10.4618423283614,52.4671311879781,11.5));
#27925=CARTESIAN_POINT('Ctrl Pts',(-10.0890808848803,52.3333605643381,11.2969997378715));
#27926=CARTESIAN_POINT('Ctrl Pts',(-10.1391162227005,52.2236363590767,11.1987310576086));
#27927=CARTESIAN_POINT('Ctrl Pts',(-10.1823079000016,52.1117651799166,11.0971961933879));
#27928=CARTESIAN_POINT('Ctrl Pts',(-10.2192535077747,52.0054502696,11.));
#27929=CARTESIAN_POINT('Ctrl Pts',(-12.0690613826432,51.9125027175599,11.2969997378715));
#27930=CARTESIAN_POINT('Ctrl Pts',(-11.9787229721437,51.8326158735901,11.1987310576086));
#27931=CARTESIAN_POINT('Ctrl Pts',(-11.8937633036688,51.7479841038615,11.0971961933879));
#27932=CARTESIAN_POINT('Ctrl Pts',(-11.8167696417768,51.6658877329441,11.));
#27933=CARTESIAN_POINT('Origin',(0.,0.,14.5));
#27934=CARTESIAN_POINT('',(-10.4618423283614,52.4671311879781,24.2));
#27935=CARTESIAN_POINT('Origin',(0.,0.,24.2));
#27936=CARTESIAN_POINT('',(-10.4618423283614,52.4671311879781,14.5));
#27937=CARTESIAN_POINT('Origin',(-10.0573948314625,52.3219895837806,14.5));
#27938=CARTESIAN_POINT('',(-9.65294733456354,52.1768479795831,24.2));
#27939=CARTESIAN_POINT('',(-9.79895497969307,52.2292448518636,24.2));
#27940=CARTESIAN_POINT('',(-9.65294733456354,52.1768479795831,11.5));
#27941=CARTESIAN_POINT('',(-9.65294733456354,52.1768479795831,14.5));
#27942=CARTESIAN_POINT('Ctrl Pts',(-9.65294733456354,52.1768479795831,11.5));
#27943=CARTESIAN_POINT('Ctrl Pts',(-9.84339863543628,52.2451940752868,11.4654707447276));
#27944=CARTESIAN_POINT('Ctrl Pts',(-10.0890808848803,52.3333605643381,11.2969997378715));
#27945=CARTESIAN_POINT('Origin',(-8.44431466907315,52.6064191384554,14.5));
#27946=CARTESIAN_POINT('',(-8.11389969301203,52.8811368237459,24.2));
#27947=CARTESIAN_POINT('',(-8.77472964513426,52.3317014531649,24.2));
#27948=CARTESIAN_POINT('',(-8.65544812419494,52.430875963113,24.2));
#27949=CARTESIAN_POINT('',(-8.11389969301203,52.8811368237459,11.5));
#27950=CARTESIAN_POINT('',(-8.11389969301203,52.8811368237459,14.5));
#27951=CARTESIAN_POINT('',(-8.41842862289464,52.6279416335077,11.2969997378715));
#27952=CARTESIAN_POINT('Ctrl Pts',(-8.11389969301203,52.8811368237459,11.5));
#27953=CARTESIAN_POINT('Ctrl Pts',(-8.26645358299714,52.7542985912954,11.3977655520826));
#27954=CARTESIAN_POINT('Ctrl Pts',(-8.41842862289464,52.6279416335077,11.2969997378715));
#27955=CARTESIAN_POINT('',(-8.77472964513426,52.3317014531649,11.5));
#27956=CARTESIAN_POINT('Ctrl Pts',(-8.41842862289464,52.6279416335077,11.2969997378715));
#27957=CARTESIAN_POINT('Ctrl Pts',(-8.61913970453336,52.4610639561783,11.4654707447276));
#27958=CARTESIAN_POINT('Ctrl Pts',(-8.77472964513426,52.3317014531649,11.5));
#27959=CARTESIAN_POINT('',(-8.77472964513426,52.3317014531649,14.5));
#27960=CARTESIAN_POINT('Origin',(0.,0.,11.25));
#27961=CARTESIAN_POINT('',(-6.77643574711567,53.0691051230866,11.5));
#27962=CARTESIAN_POINT('Origin',(0.,0.,11.5));
#27963=CARTESIAN_POINT('',(-6.413913698772,52.9096578341174,11.2969997378716));
#27964=CARTESIAN_POINT('Ctrl Pts',(-6.413913698772,52.9096578341174,11.2969997378716));
#27965=CARTESIAN_POINT('Ctrl Pts',(-6.59483018109817,52.9892299395067,11.397765552083));
#27966=CARTESIAN_POINT('Ctrl Pts',(-6.77643574711567,53.0691051230866,11.5));
#27967=CARTESIAN_POINT('Ctrl Pts',(-6.413913698772,52.9096578341174,11.2969997378716));
#27968=CARTESIAN_POINT('Ctrl Pts',(-6.47148112666752,52.8036912002342,11.1987310576087));
#27969=CARTESIAN_POINT('Ctrl Pts',(-6.5223713301853,52.6951054327476,11.0971961933879));
#27970=CARTESIAN_POINT('Ctrl Pts',(-6.56664309356486,52.5916266955276,11.));
#27971=CARTESIAN_POINT('Ctrl Pts',(-8.41842862289464,52.6279416335077,11.2969997378715));
#27972=CARTESIAN_POINT('Ctrl Pts',(-8.33388289675662,52.5419477009146,11.1987310576086));
#27973=CARTESIAN_POINT('Ctrl Pts',(-8.25503379958713,52.4515956030403,11.0971961933879));
#27974=CARTESIAN_POINT('Ctrl Pts',(-8.18395444372814,52.3643284084021,11.));
#27975=CARTESIAN_POINT('Origin',(0.,0.,14.5));
#27976=CARTESIAN_POINT('',(-6.77643574711567,53.0691051230866,24.2));
#27977=CARTESIAN_POINT('Origin',(0.,0.,24.2));
#27978=CARTESIAN_POINT('',(-6.77643574711567,53.0691051230866,14.5));
#27979=CARTESIAN_POINT('Origin',(-4.75410644754495,53.0673181599239,14.5));
#27980=CARTESIAN_POINT('',(-5.102879886332,52.8163182567097,24.2));
#27981=CARTESIAN_POINT('',(-4.97697086508332,52.9069305242525,24.2));
#27982=CARTESIAN_POINT('',(-5.102879886332,52.8163182567097,11.5));
#27983=CARTESIAN_POINT('Ctrl Pts',(-4.72678212511287,53.0869825079594,11.2969997378715));
#27984=CARTESIAN_POINT('Ctrl Pts',(-4.93864508296155,52.9345122335611,11.4654707447276));
#27985=CARTESIAN_POINT('Ctrl Pts',(-5.102879886332,52.8163182567097,11.5));
#27986=CARTESIAN_POINT('',(-5.102879886332,52.8163182567097,14.5));
#27987=CARTESIAN_POINT('Origin',(-5.60272563114623,53.3063735917395,11.));
#27988=CARTESIAN_POINT('',(-5.98976031387287,52.7231033676009,11.5));
#27989=CARTESIAN_POINT('Origin',(-5.60272563114623,53.3063735917395,11.5));
#27990=CARTESIAN_POINT('',(-5.98976031387287,52.7231033676009,24.2));
#27991=CARTESIAN_POINT('',(-5.98976031387287,52.7231033676009,14.5));
#27992=CARTESIAN_POINT('Origin',(-5.60272563114623,53.3063735917395,24.2));
#27993=CARTESIAN_POINT('Origin',(-5.60272563114623,53.3063735917395,11.25));
#27994=CARTESIAN_POINT('Ctrl Pts',(-5.98976031387287,52.7231033676009,11.5));
#27995=CARTESIAN_POINT('Ctrl Pts',(-6.1749801023183,52.8045681868194,11.4654707447276));
#27996=CARTESIAN_POINT('Ctrl Pts',(-6.413913698772,52.9096578341174,11.2969997378716));
#27997=CARTESIAN_POINT('Origin',(-6.38309803049427,52.8961042453437,14.5));
#27998=CARTESIAN_POINT('',(-6.13175727067174,52.785557582198,24.2));
#27999=CARTESIAN_POINT('Origin',(-32.9994550774553,42.2373763933203,11.25));
#28000=CARTESIAN_POINT('Origin',(-32.9994550774553,42.2373763933203,11.5));
#28001=CARTESIAN_POINT('Origin',(-29.972739626032,44.4364138889502,11.25));
#28002=CARTESIAN_POINT('Origin',(-29.972739626032,44.4364138889502,11.5));
#28003=CARTESIAN_POINT('Origin',(-26.8,46.4189616428459,11.25));
#28004=CARTESIAN_POINT('Origin',(-26.8,46.4189616428459,11.5));
#28005=CARTESIAN_POINT('Origin',(-23.4966934678946,48.1753608816354,11.25));
#28006=CARTESIAN_POINT('Origin',(-23.4966934678946,48.1753608816354,11.5));
#28007=CARTESIAN_POINT('Origin',(-20.0789134070929,49.6970546047798,11.25));
#28008=CARTESIAN_POINT('Origin',(-20.0789134070929,49.6970546047798,11.5));
#28009=CARTESIAN_POINT('Origin',(-16.5633108984972,50.9766292734202,11.25));
#28010=CARTESIAN_POINT('Origin',(-16.5633108984972,50.9766292734202,11.5));
#28011=CARTESIAN_POINT('Origin',(-12.9670136041422,52.0078509283934,11.25));
#28012=CARTESIAN_POINT('Origin',(-12.9670136041422,52.0078509283934,11.5));
#28013=CARTESIAN_POINT('Origin',(-9.30754232294747,52.7856955614544,11.25));
#28014=CARTESIAN_POINT('Origin',(-9.30754232294747,52.7856955614544,11.5));
#28015=CARTESIAN_POINT('Origin',(-9.30754232294747,52.7856955614544,11.));
#28016=CARTESIAN_POINT('Origin',(-9.30754232294747,52.7856955614544,24.2));
#28017=CARTESIAN_POINT('Origin',(-12.9670136041422,52.0078509283934,11.));
#28018=CARTESIAN_POINT('Origin',(-12.9670136041422,52.0078509283934,24.2));
#28019=CARTESIAN_POINT('Origin',(-16.5633108984972,50.9766292734202,11.));
#28020=CARTESIAN_POINT('Origin',(-16.5633108984972,50.9766292734202,24.2));
#28021=CARTESIAN_POINT('Origin',(-20.0789134070929,49.6970546047798,11.));
#28022=CARTESIAN_POINT('Origin',(-20.0789134070929,49.6970546047798,24.2));
#28023=CARTESIAN_POINT('Origin',(-23.4966934678946,48.1753608816354,11.));
#28024=CARTESIAN_POINT('Origin',(-23.4966934678946,48.1753608816354,24.2));
#28025=CARTESIAN_POINT('Origin',(-26.8,46.4189616428459,11.));
#28026=CARTESIAN_POINT('Origin',(-26.8,46.4189616428459,24.2));
#28027=CARTESIAN_POINT('Origin',(-29.972739626032,44.4364138889502,11.));
#28028=CARTESIAN_POINT('Origin',(-29.972739626032,44.4364138889502,24.2));
#28029=CARTESIAN_POINT('Origin',(-32.9994550774553,42.2373763933203,11.));
#28030=CARTESIAN_POINT('Origin',(-32.9994550774553,42.2373763933203,24.2));
#28031=CARTESIAN_POINT('Origin',(0.,0.,11.25));
#28032=CARTESIAN_POINT('',(-49.5,-6.0620016557794E-15,11.5));
#28033=CARTESIAN_POINT('Origin',(0.,0.,11.5));
#28034=CARTESIAN_POINT('',(-49.75,-6.09261782575808E-15,11.25));
#28035=CARTESIAN_POINT('Origin',(0.,0.,11.));
#28036=CARTESIAN_POINT('',(-49.5,-6.0620016557794E-15,14.5));
#28037=CARTESIAN_POINT('Origin',(0.,0.,14.5));
#28038=CARTESIAN_POINT('',(-49.5,-6.0620016557794E-15,11.));
#28039=CARTESIAN_POINT('Origin',(-51.9391184236626,11.8772792412203,14.5));
#28040=CARTESIAN_POINT('',(-51.8081802498931,11.4680127538716,24.2));
#28041=CARTESIAN_POINT('',(-51.8081802498931,11.4680127538716,14.5));
#28042=CARTESIAN_POINT('',(-51.8554496100851,11.6157600795601,24.2));
#28043=CARTESIAN_POINT('Origin',(-51.5236269022939,14.7741622717912,11.25));
#28044=CARTESIAN_POINT('Origin',(-51.5236269022939,14.7741622717912,11.5));
#28045=CARTESIAN_POINT('Origin',(-50.3675244741247,18.3322796822559,11.25));
#28046=CARTESIAN_POINT('Origin',(-50.3675244741247,18.3322796822559,11.5));
#28047=CARTESIAN_POINT('Origin',(-48.9660365296434,21.8010840688629,11.25));
#28048=CARTESIAN_POINT('Origin',(-48.9660365296434,21.8010840688629,11.5));
#28049=CARTESIAN_POINT('Origin',(-47.3259909772385,25.1636757653237,11.25));
#28050=CARTESIAN_POINT('Origin',(-47.3259909772385,25.1636757653237,11.5));
#28051=CARTESIAN_POINT('Origin',(-45.4553779539844,28.4036725628998,11.25));
#28052=CARTESIAN_POINT('Origin',(-45.4553779539844,28.4036725628998,11.5));
#28053=CARTESIAN_POINT('Origin',(-43.3633108984972,31.5052895228766,11.25));
#28054=CARTESIAN_POINT('Origin',(-43.3633108984972,31.5052895228766,11.5));
#28055=CARTESIAN_POINT('Origin',(-41.0599821511772,34.4534158791985,11.25));
#28056=CARTESIAN_POINT('Origin',(-41.0599821511772,34.4534158791985,11.5));
#28057=CARTESIAN_POINT('Origin',(-38.5566132981517,37.2336886566023,11.25));
#28058=CARTESIAN_POINT('Origin',(-38.5566132981517,37.2336886566023,11.5));
#28059=CARTESIAN_POINT('Origin',(-35.8654005008348,39.8325626455883,11.));
#28060=CARTESIAN_POINT('Origin',(-35.8654005008348,39.8325626455883,24.2));
#28061=CARTESIAN_POINT('Origin',(-38.5566132981517,37.2336886566023,11.));
#28062=CARTESIAN_POINT('Origin',(-38.5566132981517,37.2336886566023,24.2));
#28063=CARTESIAN_POINT('Origin',(-41.0599821511772,34.4534158791985,11.));
#28064=CARTESIAN_POINT('Origin',(-41.0599821511772,34.4534158791985,24.2));
#28065=CARTESIAN_POINT('Origin',(-43.3633108984972,31.5052895228766,11.));
#28066=CARTESIAN_POINT('Origin',(-43.3633108984972,31.5052895228766,24.2));
#28067=CARTESIAN_POINT('Origin',(-45.4553779539844,28.4036725628998,11.));
#28068=CARTESIAN_POINT('Origin',(-45.4553779539844,28.4036725628998,24.2));
#28069=CARTESIAN_POINT('Origin',(-47.3259909772385,25.1636757653237,11.));
#28070=CARTESIAN_POINT('Origin',(-47.3259909772385,25.1636757653237,24.2));
#28071=CARTESIAN_POINT('Origin',(-48.9660365296434,21.8010840688629,11.));
#28072=CARTESIAN_POINT('Origin',(-48.9660365296434,21.8010840688629,24.2));
#28073=CARTESIAN_POINT('Origin',(-50.3675244741247,18.3322796822559,11.));
#28074=CARTESIAN_POINT('Origin',(-50.3675244741247,18.3322796822559,24.2));
#28075=CARTESIAN_POINT('Origin',(-51.5236269022939,14.7741622717912,11.));
#28076=CARTESIAN_POINT('Origin',(-51.5236269022939,14.7741622717912,24.2));
#28077=CARTESIAN_POINT('Origin',(-52.2796703973459,10.2751081719876,14.5));
#28078=CARTESIAN_POINT('',(-52.5657520484127,9.95448198475441,24.2));
#28079=CARTESIAN_POINT('',(-52.5657520484127,9.95448198475441,14.5));
#28080=CARTESIAN_POINT('',(-51.9935887462791,10.5957343592208,24.2));
#28081=CARTESIAN_POINT('',(-52.0968657068422,10.479986641844,24.2));
#28082=CARTESIAN_POINT('',(-51.9935887462791,10.5957343592208,14.5));
#28083=CARTESIAN_POINT('Origin',(-52.428711399332,11.1440666278319,11.));
#28084=CARTESIAN_POINT('Origin',(-52.428711399332,11.1440666278319,24.2));
#28085=CARTESIAN_POINT('Origin',(-51.4355644344078,-13.8969239803295,14.5));
#28086=CARTESIAN_POINT('',(-51.7433149571624,-13.5970348695551,24.2));
#28087=CARTESIAN_POINT('',(-51.238913447339,-14.0885515659373,24.2));
#28088=CARTESIAN_POINT('',(-51.7433149571624,-13.5970348695551,11.5));
#28089=CARTESIAN_POINT('',(-51.7433149571624,-13.5970348695551,14.5));
#28090=CARTESIAN_POINT('Ctrl Pts',(-51.7433149571624,-13.597034869555,11.5));
#28091=CARTESIAN_POINT('Ctrl Pts',(-51.5386479847417,-13.7964736741256,
11.3527407245756));
#28092=CARTESIAN_POINT('Ctrl Pts',(-51.3334721998344,-13.9964082936921,
11.2067970124651));
#28093=CARTESIAN_POINT('Ctrl Pts',(-51.1278139116532,-14.196813091104,11.0622545443405));
#28094=CARTESIAN_POINT('Origin',(0.,0.,11.25));
#28095=CARTESIAN_POINT('',(-52.0700565974321,-12.286545728569,11.5));
#28096=CARTESIAN_POINT('Origin',(0.,0.,11.5));
#28097=CARTESIAN_POINT('',(-51.8081802498931,-11.4680127538716,11.0622545443405));
#28098=CARTESIAN_POINT('Ctrl Pts',(-52.0700565974321,-12.2865457285691,
11.5));
#28099=CARTESIAN_POINT('Ctrl Pts',(-51.9829772340572,-12.0143663927572,
11.3527407245753));
#28100=CARTESIAN_POINT('Ctrl Pts',(-51.8956813869633,-11.7415104052958,
11.206797012465));
#28101=CARTESIAN_POINT('Ctrl Pts',(-51.8081802498931,-11.4680127538716,
11.0622545443405));
#28102=CARTESIAN_POINT('Ctrl Pts',(-51.8081802498931,-11.4680127538716,
11.0622545443405));
#28103=CARTESIAN_POINT('Ctrl Pts',(-51.7924969656688,-11.4379708252779,
11.0404491452634));
#28104=CARTESIAN_POINT('Ctrl Pts',(-51.7780931636949,-11.4049897426814,
11.0192767711182));
#28105=CARTESIAN_POINT('Ctrl Pts',(-51.766094205967,-11.3697621197168,11.));
#28106=CARTESIAN_POINT('Origin',(-51.9391184236626,-11.8772792412203,14.5));
#28107=CARTESIAN_POINT('',(-52.0700565974321,-12.286545728569,24.2));
#28108=CARTESIAN_POINT('',(-52.0700565974321,-12.286545728569,14.5));
#28109=CARTESIAN_POINT('',(-51.8081802498931,-11.4680127538716,24.2));
#28110=CARTESIAN_POINT('',(-51.8554496100851,-11.6157600795601,24.2));
#28111=CARTESIAN_POINT('',(-51.8081802498931,-11.4680127538716,14.5));
#28112=CARTESIAN_POINT('Origin',(-52.428711399332,-11.1440666278319,11.));
#28113=CARTESIAN_POINT('',(-51.9935887462792,-10.5957343592207,24.2));
#28114=CARTESIAN_POINT('Origin',(-52.428711399332,-11.1440666278319,24.2));
#28115=CARTESIAN_POINT('',(-51.9935887462792,-10.5957343592207,11.0622545443405));
#28116=CARTESIAN_POINT('',(-51.9935887462792,-10.5957343592207,14.5));
#28117=CARTESIAN_POINT('Ctrl Pts',(-51.9151790989041,-10.6683728435365,
11.));
#28118=CARTESIAN_POINT('Ctrl Pts',(-51.9404677257214,-10.641072661922,11.0192757561174));
#28119=CARTESIAN_POINT('Ctrl Pts',(-51.967038401854,-10.6168030742446,11.0404460254343));
#28120=CARTESIAN_POINT('Ctrl Pts',(-51.9935887462792,-10.5957343592207,
11.0622545443405));
#28121=CARTESIAN_POINT('Origin',(-53.0866482765094,4.5331622039544,14.5));
#28122=CARTESIAN_POINT('',(-52.9000254978828,4.14610174160448,11.0622545443405));
#28123=CARTESIAN_POINT('',(-52.9000254978828,4.14610174160448,24.2));
#28124=CARTESIAN_POINT('',(-52.9000254978828,4.14610174160448,14.5));
#28125=CARTESIAN_POINT('',(-53.273271055136,4.92022266630433,24.2));
#28126=CARTESIAN_POINT('',(-52.9673972893853,4.28583257703743,24.2));
#28127=CARTESIAN_POINT('',(-53.2732710551359,4.92022266630433,11.5));
#28128=CARTESIAN_POINT('',(-53.2732710551359,4.92022266630433,14.5));
#28129=CARTESIAN_POINT('Ctrl Pts',(-53.2732710551359,4.92022266630432,11.5));
#28130=CARTESIAN_POINT('Ctrl Pts',(-53.1491590999574,4.66281126610928,11.3527407245754));
#28131=CARTESIAN_POINT('Ctrl Pts',(-53.024738596156,4.40475992810223,11.206797012465));
#28132=CARTESIAN_POINT('Ctrl Pts',(-52.9000254978828,4.14610174160447,11.0622545443405));
#28133=CARTESIAN_POINT('Origin',(0.,0.,11.25));
#28134=CARTESIAN_POINT('',(-53.1320940795741,6.26343186434476,11.5));
#28135=CARTESIAN_POINT('Origin',(0.,0.,11.5));
#28136=CARTESIAN_POINT('Ctrl Pts',(-53.1320940795741,6.26343186434476,11.5));
#28137=CARTESIAN_POINT('Ctrl Pts',(-52.9571754289436,6.48941388139495,11.3527407245755));
#28138=CARTESIAN_POINT('Ctrl Pts',(-52.7818219216653,6.71595770121494,11.206797012465));
#28139=CARTESIAN_POINT('Ctrl Pts',(-52.6060560429105,6.94303427461877,11.0622545443404));
#28140=CARTESIAN_POINT('Ctrl Pts',(-52.8446751870164,4.05466452110769,11.));
#28141=CARTESIAN_POINT('Ctrl Pts',(-52.8614592254452,4.08787763021397,11.0192757561174));
#28142=CARTESIAN_POINT('Ctrl Pts',(-52.8803109936724,4.11853092613597,11.0404460254343));
#28143=CARTESIAN_POINT('Ctrl Pts',(-52.9000254978828,4.14610174160448,11.0622545443405));
#28144=CARTESIAN_POINT('Origin',(-52.8690750612423,6.60323306948177,14.5));
#28145=CARTESIAN_POINT('',(-53.1320940795741,6.26343186434476,24.2));
#28146=CARTESIAN_POINT('',(-53.1320940795741,6.26343186434476,14.5));
#28147=CARTESIAN_POINT('',(-52.7010072733802,6.82036427627618,24.2));
#28148=CARTESIAN_POINT('Origin',(-53.4694330939266,3.73894699268513,11.));
#28149=CARTESIAN_POINT('',(-52.9622319224432,3.25650842494217,11.0622545443405));
#28150=CARTESIAN_POINT('Ctrl Pts',(-52.9622319224432,3.25650842494217,11.0622545443405));
#28151=CARTESIAN_POINT('Ctrl Pts',(-52.9388755042427,3.28106368122768,11.0404491452187));
#28152=CARTESIAN_POINT('Ctrl Pts',(-52.9159388628609,3.3087969065593,11.0192767711931));
#28153=CARTESIAN_POINT('Ctrl Pts',(-52.8946946754776,3.33935251029227,11.));
#28154=CARTESIAN_POINT('',(-52.9622319224432,3.25650842494217,24.2));
#28155=CARTESIAN_POINT('',(-52.9622319224432,3.25650842494217,14.5));
#28156=CARTESIAN_POINT('Origin',(-53.4694330939266,3.73894699268513,24.2));
#28157=CARTESIAN_POINT('Origin',(-52.279670397346,-10.2751081719874,14.5));
#28158=CARTESIAN_POINT('',(-52.5657520484127,-9.95448198475411,24.2));
#28159=CARTESIAN_POINT('',(-52.0968657068422,-10.479986641844,24.2));
#28160=CARTESIAN_POINT('',(-52.5657520484127,-9.95448198475412,11.5));
#28161=CARTESIAN_POINT('',(-52.5657520484127,-9.95448198475411,14.5));
#28162=CARTESIAN_POINT('Ctrl Pts',(-52.5657520484127,-9.95448198475411,
11.5));
#28163=CARTESIAN_POINT('Ctrl Pts',(-52.3754957821853,-10.167711812708,11.352740724576));
#28164=CARTESIAN_POINT('Ctrl Pts',(-52.184766529218,-10.381471740843,11.2067970124653));
#28165=CARTESIAN_POINT('Ctrl Pts',(-51.9935887462792,-10.5957343592207,
11.0622545443405));
#28166=CARTESIAN_POINT('Origin',(0.,0.,11.25));
#28167=CARTESIAN_POINT('',(-52.8002826611136,-8.62439278479999,11.5));
#28168=CARTESIAN_POINT('Origin',(0.,0.,11.5));
#28169=CARTESIAN_POINT('',(-52.4819462572372,-7.82612128585089,11.0622545443405));
#28170=CARTESIAN_POINT('Ctrl Pts',(-52.8002826611136,-8.62439278479999,
11.5));
#28171=CARTESIAN_POINT('Ctrl Pts',(-52.6944291479996,-8.35895081349672,
11.352740724576));
#28172=CARTESIAN_POINT('Ctrl Pts',(-52.5883124776762,-8.09284893997223,
11.2067970124653));
#28173=CARTESIAN_POINT('Ctrl Pts',(-52.4819462572372,-7.82612128585088,
11.0622545443405));
#28174=CARTESIAN_POINT('Ctrl Pts',(-52.4819462572372,-7.82612128585089,
11.0622545443405));
#28175=CARTESIAN_POINT('Ctrl Pts',(-52.4642055576654,-7.79724654843031,
11.0404491452187));
#28176=CARTESIAN_POINT('Ctrl Pts',(-52.4475361986995,-7.76535056472022,
11.0192767711931));
#28177=CARTESIAN_POINT('Ctrl Pts',(-52.4331091150171,-7.73104575932095,
11.));
#28178=CARTESIAN_POINT('Origin',(-52.6411144591754,-8.22525703532544,14.5));
#28179=CARTESIAN_POINT('',(-52.8002826611136,-8.62439278479999,24.2));
#28180=CARTESIAN_POINT('',(-52.8002826611136,-8.62439278479999,14.5));
#28181=CARTESIAN_POINT('',(-52.4819462572372,-7.82612128585089,24.2));
#28182=CARTESIAN_POINT('',(-52.5394068040886,-7.97021136259661,24.2));
#28183=CARTESIAN_POINT('',(-52.4819462572372,-7.82612128585089,14.5));
#28184=CARTESIAN_POINT('Origin',(-53.0783684845482,-7.45967821145951,11.));
#28185=CARTESIAN_POINT('',(-52.6060560429105,-6.94303427461878,24.2));
#28186=CARTESIAN_POINT('Origin',(-53.0783684845482,-7.45967821145951,24.2));
#28187=CARTESIAN_POINT('',(-52.6060560429105,-6.94303427461879,11.0622545443404));
#28188=CARTESIAN_POINT('',(-52.6060560429105,-6.94303427461879,14.5));
#28189=CARTESIAN_POINT('Ctrl Pts',(-52.5329044020197,-7.02096539574592,
11.));
#28190=CARTESIAN_POINT('Ctrl Pts',(-52.556227062611,-6.9919676705692,11.0192757561174));
#28191=CARTESIAN_POINT('Ctrl Pts',(-52.5810400530563,-6.96590372571557,
11.0404460254343));
#28192=CARTESIAN_POINT('Ctrl Pts',(-52.6060560429105,-6.94303427461878,
11.0622545443404));
#28193=CARTESIAN_POINT('Origin',(-53.2735492796914,0.818982261997372,14.5));
#28194=CARTESIAN_POINT('',(-53.0603811317945,0.445882806437586,11.0622545443404));
#28195=CARTESIAN_POINT('',(-53.0603811317945,0.445882806437586,24.2));
#28196=CARTESIAN_POINT('',(-53.0603811317945,0.445882806437586,14.5));
#28197=CARTESIAN_POINT('',(-53.4867174275882,1.19208171755716,24.2));
#28198=CARTESIAN_POINT('',(-53.1373359393522,0.580573645973276,24.2));
#28199=CARTESIAN_POINT('',(-53.4867174275882,1.19208171755716,11.5));
#28200=CARTESIAN_POINT('',(-53.4867174275882,1.19208171755716,14.5));
#28201=CARTESIAN_POINT('Ctrl Pts',(-53.4867174275882,1.19208171755716,11.5));
#28202=CARTESIAN_POINT('Ctrl Pts',(-53.3449516913153,0.943954970938035,
11.3527407245752));
#28203=CARTESIAN_POINT('Ctrl Pts',(-53.2028335182235,0.69521136862767,11.2067970124649));
#28204=CARTESIAN_POINT('Ctrl Pts',(-53.0603811317945,0.445882806437587,
11.0622545443404));
#28205=CARTESIAN_POINT('Origin',(0.,0.,11.25));
#28206=CARTESIAN_POINT('',(-53.4395818891992,2.5418669334897,11.5));
#28207=CARTESIAN_POINT('Origin',(0.,0.,11.5));
#28208=CARTESIAN_POINT('Ctrl Pts',(-53.4395818891992,2.54186693348971,11.5));
#28209=CARTESIAN_POINT('Ctrl Pts',(-53.280853040249,2.77950017796476,11.3527407245753));
#28210=CARTESIAN_POINT('Ctrl Pts',(-53.1217295833205,3.01772419075198,11.206797012465));
#28211=CARTESIAN_POINT('Ctrl Pts',(-52.9622319224432,3.25650842494217,11.0622545443405));
#28212=CARTESIAN_POINT('Ctrl Pts',(-52.9987873134328,0.35852936492104,11.));
#28213=CARTESIAN_POINT('Ctrl Pts',(-53.0178472961609,0.390490773226822,
11.0192757561174));
#28214=CARTESIAN_POINT('Ctrl Pts',(-53.0387914082603,0.419754366385184,
11.0404460254343));
#28215=CARTESIAN_POINT('Ctrl Pts',(-53.0603811317945,0.445882806437586,
11.0622545443404));
#28216=CARTESIAN_POINT('Origin',(-53.2009069058212,2.89918767921594,14.5));
#28217=CARTESIAN_POINT('',(-53.4395818891992,2.5418669334897,24.2));
#28218=CARTESIAN_POINT('',(-53.4395818891992,2.5418669334897,14.5));
#28219=CARTESIAN_POINT('',(-53.048394829969,3.12751378153497,24.2));
#28220=CARTESIAN_POINT('Origin',(-53.6,6.56410684342981E-15,11.));
#28221=CARTESIAN_POINT('',(-53.0603811317945,-0.445882806437573,11.0622545443404));
#28222=CARTESIAN_POINT('Ctrl Pts',(-53.0603811317945,-0.445882806437573,
11.0622545443404));
#28223=CARTESIAN_POINT('Ctrl Pts',(-53.0387944967453,-0.419758104149289,
11.0404491452186));
#28224=CARTESIAN_POINT('Ctrl Pts',(-53.0178482998738,-0.390492456338415,
11.0192767711931));
#28225=CARTESIAN_POINT('Ctrl Pts',(-52.9987873134328,-0.358529364921027,
11.));
#28226=CARTESIAN_POINT('',(-53.0603811317945,-0.445882806437573,24.2));
#28227=CARTESIAN_POINT('',(-53.0603811317945,-0.445882806437573,14.5));
#28228=CARTESIAN_POINT('Origin',(-53.6,6.56410684342981E-15,24.2));
#28229=CARTESIAN_POINT('Origin',(-52.8690750612423,-6.60323306948178,14.5));
#28230=CARTESIAN_POINT('',(-53.1320940795741,-6.26343186434478,24.2));
#28231=CARTESIAN_POINT('',(-52.7010072733802,-6.82036427627619,24.2));
#28232=CARTESIAN_POINT('',(-53.1320940795741,-6.26343186434478,11.5));
#28233=CARTESIAN_POINT('',(-53.1320940795741,-6.26343186434477,14.5));
#28234=CARTESIAN_POINT('Ctrl Pts',(-53.1320940795741,-6.26343186434478,
11.5));
#28235=CARTESIAN_POINT('Ctrl Pts',(-52.9571754289434,-6.48941388139521,
11.3527407245754));
#28236=CARTESIAN_POINT('Ctrl Pts',(-52.7818219216652,-6.71595770121507,
11.206797012465));
#28237=CARTESIAN_POINT('Ctrl Pts',(-52.6060560429105,-6.94303427461878,
11.0622545443404));
#28238=CARTESIAN_POINT('Origin',(0.,0.,11.25));
#28239=CARTESIAN_POINT('',(-53.273271055136,-4.920222666304,11.5));
#28240=CARTESIAN_POINT('Origin',(0.,0.,11.5));
#28241=CARTESIAN_POINT('',(-52.9000254978827,-4.1461017416044,11.0622545443404));
#28242=CARTESIAN_POINT('Ctrl Pts',(-53.273271055136,-4.920222666304,11.5));
#28243=CARTESIAN_POINT('Ctrl Pts',(-53.1491590999572,-4.6628112661087,11.3527407245752));
#28244=CARTESIAN_POINT('Ctrl Pts',(-53.0247385961559,-4.40475992810191,
11.2067970124649));
#28245=CARTESIAN_POINT('Ctrl Pts',(-52.9000254978827,-4.1461017416044,11.0622545443404));
#28246=CARTESIAN_POINT('Ctrl Pts',(-52.9000254978827,-4.1461017416044,11.0622545443404));
#28247=CARTESIAN_POINT('Ctrl Pts',(-52.8803138139007,-4.11853487023683,
11.0404491452186));
#28248=CARTESIAN_POINT('Ctrl Pts',(-52.8614601093052,-4.08787937924104,
11.0192767711931));
#28249=CARTESIAN_POINT('Ctrl Pts',(-52.8446751870164,-4.05466452110769,
11.));
#28250=CARTESIAN_POINT('Origin',(-53.0866482765093,-4.5331622039542,14.5));
#28251=CARTESIAN_POINT('',(-53.273271055136,-4.920222666304,24.2));
#28252=CARTESIAN_POINT('',(-53.273271055136,-4.920222666304,14.5));
#28253=CARTESIAN_POINT('',(-52.9000254978827,-4.1461017416044,24.2));
#28254=CARTESIAN_POINT('',(-52.9673972893853,-4.2858325770374,24.2));
#28255=CARTESIAN_POINT('',(-52.9000254978827,-4.1461017416044,14.5));
#28256=CARTESIAN_POINT('Origin',(-53.4694330939266,-3.73894699268512,11.));
#28257=CARTESIAN_POINT('',(-52.9622319224432,-3.25650842494215,24.2));
#28258=CARTESIAN_POINT('Origin',(-53.4694330939266,-3.73894699268512,24.2));
#28259=CARTESIAN_POINT('',(-52.9622319224432,-3.25650842494215,11.0622545443405));
#28260=CARTESIAN_POINT('',(-52.9622319224432,-3.25650842494215,14.5));
#28261=CARTESIAN_POINT('Ctrl Pts',(-52.8946946754777,-3.33935251029225,
11.));
#28262=CARTESIAN_POINT('Ctrl Pts',(-52.9159377441851,-3.30879851555543,
11.0192757561174));
#28263=CARTESIAN_POINT('Ctrl Pts',(-52.9388721625479,-3.28106719444495,
11.0404460254343));
#28264=CARTESIAN_POINT('Ctrl Pts',(-52.9622319224432,-3.25650842494215,
11.0622545443405));
#28265=CARTESIAN_POINT('Origin',(-53.2009069058212,-2.89918767921592,14.5));
#28266=CARTESIAN_POINT('',(-53.4395818891992,-2.54186693348969,24.2));
#28267=CARTESIAN_POINT('',(-53.048394829969,-3.12751378153496,24.2));
#28268=CARTESIAN_POINT('',(-53.4395818891992,-2.54186693348969,11.5));
#28269=CARTESIAN_POINT('',(-53.4395818891992,-2.54186693348969,14.5));
#28270=CARTESIAN_POINT('Ctrl Pts',(-53.4395818891992,-2.54186693348969,
11.5));
#28271=CARTESIAN_POINT('Ctrl Pts',(-53.280853040249,-2.7795001779648,11.3527407245752));
#28272=CARTESIAN_POINT('Ctrl Pts',(-53.1217295833205,-3.01772419075199,
11.2067970124649));
#28273=CARTESIAN_POINT('Ctrl Pts',(-52.9622319224432,-3.25650842494215,
11.0622545443405));
#28274=CARTESIAN_POINT('Origin',(0.,0.,11.25));
#28275=CARTESIAN_POINT('',(-53.4867174275882,-1.19208171755714,11.5));
#28276=CARTESIAN_POINT('Origin',(0.,0.,11.5));
#28277=CARTESIAN_POINT('Ctrl Pts',(-53.4867174275882,-1.19208171755715,
11.5));
#28278=CARTESIAN_POINT('Ctrl Pts',(-53.3449516913151,-0.943954970937745,
11.3527407245751));
#28279=CARTESIAN_POINT('Ctrl Pts',(-53.2028335182234,-0.695211368627523,
11.2067970124648));
#28280=CARTESIAN_POINT('Ctrl Pts',(-53.0603811317945,-0.445882806437576,
11.0622545443404));
#28281=CARTESIAN_POINT('Origin',(-53.2735492796914,-0.818982261997359,14.5));
#28282=CARTESIAN_POINT('',(-53.4867174275882,-1.19208171755714,24.2));
#28283=CARTESIAN_POINT('',(-53.4867174275882,-1.19208171755714,14.5));
#28284=CARTESIAN_POINT('',(-53.1373359393522,-0.580573645973263,24.2));
#28285=CARTESIAN_POINT('Origin',(0.,-1.62429660857958E-15,24.8232233047034));
#28286=CARTESIAN_POINT('',(-53.0535533905933,-1.29943728686367E-14,24.6464466094067));
#28287=CARTESIAN_POINT('Origin',(0.,-3.24859321715916E-15,24.6464466094067));
#28288=CARTESIAN_POINT('',(-52.2,6.39265629154918E-15,25.));
#28289=CARTESIAN_POINT('',(-52.6267766952966,3.19632814577459E-15,24.8232233047034));
#28290=CARTESIAN_POINT('Origin',(0.,0.,25.));
#28291=CARTESIAN_POINT('Origin',(0.,0.,25.));
#28292=CARTESIAN_POINT('',(-51.1,-6.25794514364297E-15,25.));
#28293=CARTESIAN_POINT('Origin',(0.,0.,25.));
#28294=CARTESIAN_POINT('Origin',(0.,0.,24.6));
#28295=CARTESIAN_POINT('',(-53.5,-6.55186037543834E-15,24.2));
#28296=CARTESIAN_POINT('',(-53.1,-6.50287450347244E-15,24.6));
#28297=CARTESIAN_POINT('Origin',(0.,0.,24.2));
#28298=CARTESIAN_POINT('Origin',(0.,0.,24.2));
#28299=CARTESIAN_POINT('Origin',(0.,0.,24.2));
#28300=CARTESIAN_POINT('Origin',(0.,0.,24.2));
#28301=CARTESIAN_POINT('Origin',(0.,0.,24.2));
#28302=CARTESIAN_POINT('Origin',(0.,0.,24.2));
#28303=CARTESIAN_POINT('Origin',(0.,0.,24.2));
#28304=CARTESIAN_POINT('Origin',(0.,0.,24.2));
#28305=CARTESIAN_POINT('Origin',(0.,0.,24.2));
#28306=CARTESIAN_POINT('Origin',(0.,0.,24.2));
#28307=CARTESIAN_POINT('Origin',(0.,0.,24.2));
#28308=CARTESIAN_POINT('Origin',(0.,0.,24.2));
#28309=CARTESIAN_POINT('Origin',(0.,0.,24.2));
#28310=CARTESIAN_POINT('Origin',(0.,0.,24.2));
#28311=CARTESIAN_POINT('Origin',(0.,0.,24.2));
#28312=CARTESIAN_POINT('Origin',(0.,0.,24.2));
#28313=CARTESIAN_POINT('Origin',(0.,0.,24.2));
#28314=CARTESIAN_POINT('Origin',(0.,0.,24.2));
#28315=CARTESIAN_POINT('Origin',(0.,0.,24.2));
#28316=CARTESIAN_POINT('Origin',(0.,0.,24.2));
#28317=CARTESIAN_POINT('Origin',(0.,0.,24.2));
#28318=CARTESIAN_POINT('Origin',(0.,0.,24.2));
#28319=CARTESIAN_POINT('Origin',(0.,0.,24.2));
#28320=CARTESIAN_POINT('Origin',(0.,0.,24.2));
#28321=CARTESIAN_POINT('Origin',(0.,0.,24.2));
#28322=CARTESIAN_POINT('Origin',(0.,0.,24.2));
#28323=CARTESIAN_POINT('Origin',(0.,0.,24.2));
#28324=CARTESIAN_POINT('Origin',(0.,0.,24.2));
#28325=CARTESIAN_POINT('Origin',(0.,0.,24.2));
#28326=CARTESIAN_POINT('Origin',(0.,0.,24.2));
#28327=CARTESIAN_POINT('Origin',(0.,0.,24.2));
#28328=CARTESIAN_POINT('Origin',(0.,0.,24.2));
#28329=CARTESIAN_POINT('Origin',(0.,0.,24.2));
#28330=CARTESIAN_POINT('Origin',(0.,0.,24.2));
#28331=CARTESIAN_POINT('Origin',(0.,0.,24.2));
#28332=CARTESIAN_POINT('Origin',(0.,0.,24.2));
#28333=CARTESIAN_POINT('Origin',(0.,0.,24.2));
#28334=CARTESIAN_POINT('Origin',(0.,0.,24.2));
#28335=CARTESIAN_POINT('Origin',(0.,0.,24.2));
#28336=CARTESIAN_POINT('Origin',(0.,0.,24.2));
#28337=CARTESIAN_POINT('Origin',(0.,0.,24.2));
#28338=CARTESIAN_POINT('Origin',(0.,0.,24.2));
#28339=CARTESIAN_POINT('Origin',(0.,0.,24.2));
#28340=CARTESIAN_POINT('Origin',(0.,0.,24.2));
#28341=CARTESIAN_POINT('Origin',(0.,0.,24.2));
#28342=CARTESIAN_POINT('Origin',(0.,0.,24.2));
#28343=CARTESIAN_POINT('Origin',(0.,0.,24.2));
#28344=CARTESIAN_POINT('Origin',(0.,0.,24.2));
#28345=CARTESIAN_POINT('Origin',(0.,0.,24.2));
#28346=CARTESIAN_POINT('Origin',(0.,0.,24.2));
#28347=CARTESIAN_POINT('Origin',(0.,0.,24.2));
#28348=CARTESIAN_POINT('Origin',(0.,0.,24.2));
#28349=CARTESIAN_POINT('Origin',(0.,0.,24.2));
#28350=CARTESIAN_POINT('Origin',(0.,0.,24.2));
#28351=CARTESIAN_POINT('Origin',(0.,0.,24.2));
#28352=CARTESIAN_POINT('Origin',(0.,0.,24.2));
#28353=CARTESIAN_POINT('Origin',(0.,0.,24.2));
#28354=CARTESIAN_POINT('Origin',(0.,0.,24.2));
#28355=CARTESIAN_POINT('Origin',(0.,0.,24.2));
#28356=CARTESIAN_POINT('Origin',(0.,0.,24.2));
#28357=CARTESIAN_POINT('Origin',(0.,0.,24.2));
#28358=CARTESIAN_POINT('Origin',(0.,0.,24.2));
#28359=CARTESIAN_POINT('Origin',(0.,0.,24.2));
#28360=CARTESIAN_POINT('Origin',(0.,0.,24.2));
#28361=CARTESIAN_POINT('Origin',(0.,0.,24.2));
#28362=CARTESIAN_POINT('Origin',(0.,0.,24.2));
#28363=CARTESIAN_POINT('Origin',(0.,0.,24.2));
#28364=CARTESIAN_POINT('Origin',(0.,0.,24.2));
#28365=CARTESIAN_POINT('Origin',(0.,0.,24.2));
#28366=CARTESIAN_POINT('Origin',(0.,0.,24.2));
#28367=CARTESIAN_POINT('Origin',(0.,0.,24.2));
#28368=CARTESIAN_POINT('Origin',(0.,0.,24.2));
#28369=CARTESIAN_POINT('Origin',(0.,0.,24.2));
#28370=CARTESIAN_POINT('Origin',(0.,0.,24.2));
#28371=CARTESIAN_POINT('Origin',(0.,0.,24.2));
#28372=CARTESIAN_POINT('Origin',(0.,0.,24.2));
#28373=CARTESIAN_POINT('Origin',(0.,0.,24.2));
#28374=CARTESIAN_POINT('Origin',(0.,0.,24.2));
#28375=CARTESIAN_POINT('Origin',(0.,0.,24.2));
#28376=CARTESIAN_POINT('Origin',(0.,0.,24.2));
#28377=CARTESIAN_POINT('Origin',(0.,0.,24.2));
#28378=CARTESIAN_POINT('Origin',(0.,0.,24.2));
#28379=CARTESIAN_POINT('Origin',(0.,0.,24.2));
#28380=CARTESIAN_POINT('Origin',(0.,0.,24.2));
#28381=CARTESIAN_POINT('Origin',(0.,0.,24.2));
#28382=CARTESIAN_POINT('Origin',(0.,0.,24.2));
#28383=CARTESIAN_POINT('Origin',(0.,0.,24.2));
#28384=CARTESIAN_POINT('Origin',(0.,0.,24.2));
#28385=CARTESIAN_POINT('Origin',(0.,0.,24.2));
#28386=CARTESIAN_POINT('Origin',(0.,0.,24.2));
#28387=CARTESIAN_POINT('Origin',(0.,0.,24.2));
#28388=CARTESIAN_POINT('Origin',(0.,0.,24.2));
#28389=CARTESIAN_POINT('Origin',(0.,0.,24.2));
#28390=CARTESIAN_POINT('Origin',(0.,0.,24.2));
#28391=CARTESIAN_POINT('Origin',(0.,0.,24.2));
#28392=CARTESIAN_POINT('Origin',(0.,0.,24.2));
#28393=CARTESIAN_POINT('Origin',(0.,0.,24.2));
#28394=CARTESIAN_POINT('Origin',(0.,0.,24.2));
#28395=CARTESIAN_POINT('Origin',(0.,0.,24.2));
#28396=CARTESIAN_POINT('Origin',(0.,0.,24.2));
#28397=CARTESIAN_POINT('Origin',(0.,0.,24.2));
#28398=CARTESIAN_POINT('Origin',(9.57952682562336,-29.4827520051498,22.3));
#28399=CARTESIAN_POINT('',(-3.32047317437664,-29.4827520051498,22.5));
#28400=CARTESIAN_POINT('Origin',(9.57952682562336,-29.4827520051498,22.5));
#28401=CARTESIAN_POINT('',(-2.92047317437664,-29.4827520051498,22.1));
#28402=CARTESIAN_POINT('',(-3.12047317437664,-29.4827520051498,22.3));
#28403=CARTESIAN_POINT('Origin',(9.57952682562336,-29.4827520051498,22.1));
#28404=CARTESIAN_POINT('Origin',(0.,0.,22.5));
#28405=CARTESIAN_POINT('',(-50.5,-6.18446633569413E-15,22.5));
#28406=CARTESIAN_POINT('Origin',(0.,0.,22.5));
#28407=CARTESIAN_POINT('',(18.1,-1.57979437090009E-15,22.5));
#28408=CARTESIAN_POINT('Origin',(31.,0.,22.5));
#28409=CARTESIAN_POINT('',(-37.9795268256234,18.2213428210667,22.5));
#28410=CARTESIAN_POINT('Origin',(-25.0795268256234,18.2213428210667,22.5));
#28411=CARTESIAN_POINT('',(-5.025,-6.15385016571545E-16,22.5));
#28412=CARTESIAN_POINT('Origin',(0.,0.,22.5));
#28413=CARTESIAN_POINT('',(-37.9795268256234,-18.2213428210667,22.5));
#28414=CARTESIAN_POINT('Origin',(-25.0795268256234,-18.2213428210667,22.5));
#28415=CARTESIAN_POINT('',(-3.32047317437663,29.4827520051498,22.5));
#28416=CARTESIAN_POINT('Origin',(9.57952682562337,29.4827520051498,22.5));
#28417=CARTESIAN_POINT('Origin',(9.57952682562336,-29.4827520051498,22.5));
#28418=CARTESIAN_POINT('',(-2.92047317437664,-29.4827520051498,14.5));
#28419=CARTESIAN_POINT('',(-2.92047317437664,-29.4827520051498,22.5));
#28420=CARTESIAN_POINT('Origin',(9.57952682562336,-29.4827520051498,14.5));
#28421=CARTESIAN_POINT('Origin',(31.,0.,22.3));
#28422=CARTESIAN_POINT('',(18.5,1.53080849893419E-15,22.1));
#28423=CARTESIAN_POINT('',(18.3,-1.55530143491714E-15,22.3));
#28424=CARTESIAN_POINT('Origin',(31.,0.,22.1));
#28425=CARTESIAN_POINT('Origin',(31.,0.,22.5));
#28426=CARTESIAN_POINT('',(18.5,-1.53080849893419E-15,14.5));
#28427=CARTESIAN_POINT('',(18.5,1.53080849893419E-15,22.5));
#28428=CARTESIAN_POINT('Origin',(31.,0.,14.5));
#28429=CARTESIAN_POINT('Origin',(9.57952682562337,29.4827520051498,22.3));
#28430=CARTESIAN_POINT('',(-2.92047317437663,29.4827520051498,22.1));
#28431=CARTESIAN_POINT('',(-3.12047317437663,29.4827520051498,22.3));
#28432=CARTESIAN_POINT('Origin',(9.57952682562337,29.4827520051498,22.1));
#28433=CARTESIAN_POINT('Origin',(9.57952682562337,29.4827520051498,22.5));
#28434=CARTESIAN_POINT('',(-2.92047317437663,29.4827520051498,14.5));
#28435=CARTESIAN_POINT('',(-2.92047317437663,29.4827520051498,22.5));
#28436=CARTESIAN_POINT('Origin',(9.57952682562337,29.4827520051498,14.5));
#28437=CARTESIAN_POINT('Origin',(-25.0795268256234,18.2213428210667,22.3));
#28438=CARTESIAN_POINT('',(-37.5795268256234,18.2213428210667,22.1));
#28439=CARTESIAN_POINT('',(-37.7795268256234,18.2213428210667,22.3));
#28440=CARTESIAN_POINT('Origin',(-25.0795268256234,18.2213428210667,22.1));
#28441=CARTESIAN_POINT('Origin',(-25.0795268256234,18.2213428210667,22.5));
#28442=CARTESIAN_POINT('',(-37.5795268256234,18.2213428210667,14.5));
#28443=CARTESIAN_POINT('',(-37.5795268256234,18.2213428210667,22.5));
#28444=CARTESIAN_POINT('Origin',(-25.0795268256234,18.2213428210667,14.5));
#28445=CARTESIAN_POINT('Origin',(-25.0795268256234,-18.2213428210667,22.3));
#28446=CARTESIAN_POINT('',(-37.5795268256234,-18.2213428210667,22.1));
#28447=CARTESIAN_POINT('',(-37.7795268256234,-18.2213428210667,22.3));
#28448=CARTESIAN_POINT('Origin',(-25.0795268256234,-18.2213428210667,22.1));
#28449=CARTESIAN_POINT('Origin',(-25.0795268256234,-18.2213428210667,22.5));
#28450=CARTESIAN_POINT('',(-37.5795268256234,-18.2213428210667,14.5));
#28451=CARTESIAN_POINT('',(-37.5795268256234,-18.2213428210667,22.5));
#28452=CARTESIAN_POINT('Origin',(-25.0795268256234,-18.2213428210667,14.5));
#28453=CARTESIAN_POINT('Origin',(0.,0.,24.7));
#28454=CARTESIAN_POINT('',(-50.5,6.18446633569413E-15,24.4));
#28455=CARTESIAN_POINT('',(-50.8,-6.22120573966855E-15,24.7));
#28456=CARTESIAN_POINT('Origin',(0.,0.,24.4));
#28457=CARTESIAN_POINT('Origin',(0.,0.,22.5));
#28458=CARTESIAN_POINT('',(-50.5,-6.18446633569413E-15,22.5));
#28459=CARTESIAN_POINT('Origin',(0.,0.,14.5));
#28460=CARTESIAN_POINT('Origin',(0.,0.,14.5));
#28461=CARTESIAN_POINT('Origin',(0.,0.,14.5));
#28462=CARTESIAN_POINT('Origin',(0.,0.,14.5));
#28463=CARTESIAN_POINT('Origin',(0.,0.,14.5));
#28464=CARTESIAN_POINT('Origin',(0.,0.,14.5));
#28465=CARTESIAN_POINT('Origin',(0.,0.,14.5));
#28466=CARTESIAN_POINT('Origin',(0.,0.,14.5));
#28467=CARTESIAN_POINT('Origin',(0.,0.,14.5));
#28468=CARTESIAN_POINT('Origin',(0.,0.,14.5));
#28469=CARTESIAN_POINT('Origin',(53.4694330939266,-3.73894699268513,24.2));
#28470=CARTESIAN_POINT('Origin',(53.0783684845482,-7.45967821145953,24.2));
#28471=CARTESIAN_POINT('Origin',(52.428711399332,-11.1440666278319,24.2));
#28472=CARTESIAN_POINT('Origin',(51.5236269022939,-14.7741622717911,24.2));
#28473=CARTESIAN_POINT('Origin',(50.3675244741247,-18.3322796822558,24.2));
#28474=CARTESIAN_POINT('Origin',(48.9660365296434,-21.8010840688629,24.2));
#28475=CARTESIAN_POINT('Origin',(47.3259909772385,-25.1636757653237,11.));
#28476=CARTESIAN_POINT('Origin',(47.3259909772385,-25.1636757653237,24.2));
#28477=CARTESIAN_POINT('Origin',(47.3259909772385,-25.1636757653237,24.2));
#28478=CARTESIAN_POINT('Origin',(45.4553779539844,-28.4036725628998,24.2));
#28479=CARTESIAN_POINT('Origin',(43.3633108984972,-31.5052895228766,24.2));
#28480=CARTESIAN_POINT('Origin',(41.0599821511772,-34.4534158791985,24.2));
#28481=CARTESIAN_POINT('Origin',(38.5566132981517,-37.2336886566023,24.2));
#28482=CARTESIAN_POINT('Origin',(35.8654005008348,-39.8325626455884,24.2));
#28483=CARTESIAN_POINT('Origin',(32.9994550774553,-42.2373763933203,24.2));
#28484=CARTESIAN_POINT('Origin',(29.972739626032,-44.4364138889502,24.2));
#28485=CARTESIAN_POINT('Origin',(26.8,-46.4189616428459,24.2));
#28486=CARTESIAN_POINT('Origin',(23.4966934678945,-48.1753608816354,24.2));
#28487=CARTESIAN_POINT('Origin',(20.0789134070929,-49.6970546047798,11.));
#28488=CARTESIAN_POINT('Origin',(20.0789134070929,-49.6970546047798,24.2));
#28489=CARTESIAN_POINT('Origin',(20.0789134070929,-49.6970546047798,24.2));
#28490=CARTESIAN_POINT('Origin',(16.5633108984972,-50.9766292734202,24.2));
#28491=CARTESIAN_POINT('Origin',(12.9670136041422,-52.0078509283934,24.2));
#28492=CARTESIAN_POINT('Origin',(9.30754232294745,-52.7856955614544,24.2));
#28493=CARTESIAN_POINT('Origin',(5.6027256311462,-53.3063735917395,24.2));
#28494=CARTESIAN_POINT('Origin',(1.87061302325407,-53.5673483282235,24.2));
#28495=CARTESIAN_POINT('Origin',(-1.87061302325404,-53.5673483282235,24.2));
#28496=CARTESIAN_POINT('Origin',(-5.60272563114622,-53.3063735917395,24.2));
#28497=CARTESIAN_POINT('Origin',(-9.30754232294747,-52.7856955614544,24.2));
#28498=CARTESIAN_POINT('Origin',(-12.9670136041422,-52.0078509283934,24.2));
#28499=CARTESIAN_POINT('Origin',(-16.5633108984972,-50.9766292734202,11.));
#28500=CARTESIAN_POINT('Origin',(-16.5633108984972,-50.9766292734202,24.2));
#28501=CARTESIAN_POINT('Origin',(-16.5633108984972,-50.9766292734202,24.2));
#28502=CARTESIAN_POINT('Origin',(-20.0789134070929,-49.6970546047798,24.2));
#28503=CARTESIAN_POINT('Origin',(-23.4966934678946,-48.1753608816353,24.2));
#28504=CARTESIAN_POINT('Origin',(-26.8,-46.4189616428459,24.2));
#28505=CARTESIAN_POINT('Origin',(-29.972739626032,-44.4364138889502,24.2));
#28506=CARTESIAN_POINT('Origin',(-32.9994550774553,-42.2373763933203,24.2));
#28507=CARTESIAN_POINT('Origin',(-35.8654005008348,-39.8325626455883,24.2));
#28508=CARTESIAN_POINT('Origin',(-38.5566132981517,-37.2336886566023,24.2));
#28509=CARTESIAN_POINT('Origin',(-41.0599821511772,-34.4534158791985,24.2));
#28510=CARTESIAN_POINT('Origin',(-43.3633108984972,-31.5052895228766,24.2));
#28511=CARTESIAN_POINT('Origin',(-45.4553779539844,-28.4036725628998,24.2));
#28512=CARTESIAN_POINT('Origin',(-47.3259909772385,-25.1636757653237,24.2));
#28513=CARTESIAN_POINT('Origin',(-48.9660365296434,-21.8010840688629,24.2));
#28514=CARTESIAN_POINT('Origin',(-50.3675244741247,-18.3322796822558,24.2));
#28515=CARTESIAN_POINT('Origin',(-51.5236269022939,-14.7741622717911,24.2));
#28516=CARTESIAN_POINT('Origin',(-52.428711399332,-11.1440666278319,24.2));
#28517=CARTESIAN_POINT('Origin',(-53.0783684845482,-7.45967821145951,24.2));
#28518=CARTESIAN_POINT('Origin',(-53.4694330939266,-3.73894699268512,24.2));
#28519=CARTESIAN_POINT('Origin',(-53.6,6.56410684342981E-15,24.2));
#28520=CARTESIAN_POINT('Origin',(-53.4694330939266,3.73894699268513,24.2));
#28521=CARTESIAN_POINT('Origin',(-53.0783684845482,7.4596782114595,24.2));
#28522=CARTESIAN_POINT('Origin',(-52.428711399332,11.1440666278319,24.2));
#28523=CARTESIAN_POINT('Origin',(-51.5236269022939,14.7741622717912,24.2));
#28524=CARTESIAN_POINT('Origin',(-50.3675244741247,18.3322796822559,24.2));
#28525=CARTESIAN_POINT('Origin',(-48.9660365296434,21.8010840688629,24.2));
#28526=CARTESIAN_POINT('Origin',(-47.3259909772385,25.1636757653237,24.2));
#28527=CARTESIAN_POINT('Origin',(-45.4553779539844,28.4036725628998,24.2));
#28528=CARTESIAN_POINT('Origin',(-43.3633108984972,31.5052895228766,24.2));
#28529=CARTESIAN_POINT('Origin',(-41.0599821511772,34.4534158791985,24.2));
#28530=CARTESIAN_POINT('Origin',(-38.5566132981517,37.2336886566023,24.2));
#28531=CARTESIAN_POINT('Origin',(-35.8654005008348,39.8325626455883,24.2));
#28532=CARTESIAN_POINT('Origin',(-32.9994550774553,42.2373763933203,24.2));
#28533=CARTESIAN_POINT('Origin',(-29.972739626032,44.4364138889502,24.2));
#28534=CARTESIAN_POINT('Origin',(-26.8,46.4189616428459,24.2));
#28535=CARTESIAN_POINT('Origin',(-23.4966934678946,48.1753608816354,24.2));
#28536=CARTESIAN_POINT('Origin',(-20.0789134070929,49.6970546047798,24.2));
#28537=CARTESIAN_POINT('Origin',(-16.5633108984972,50.9766292734202,24.2));
#28538=CARTESIAN_POINT('Origin',(-12.9670136041422,52.0078509283934,24.2));
#28539=CARTESIAN_POINT('Origin',(-9.30754232294747,52.7856955614544,24.2));
#28540=CARTESIAN_POINT('Origin',(-5.60272563114623,53.3063735917395,24.2));
#28541=CARTESIAN_POINT('Origin',(-1.87061302325405,53.5673483282235,24.2));
#28542=CARTESIAN_POINT('Origin',(-1.87061302325405,53.5673483282235,24.2));
#28543=CARTESIAN_POINT('Origin',(-1.87061302325405,53.5673483282235,11.));
#28544=CARTESIAN_POINT('Origin',(1.87061302325406,53.5673483282235,24.2));
#28545=CARTESIAN_POINT('Origin',(5.60272563114623,53.3063735917395,24.2));
#28546=CARTESIAN_POINT('Origin',(9.30754232294747,52.7856955614544,24.2));
#28547=CARTESIAN_POINT('Origin',(12.9670136041422,52.0078509283934,24.2));
#28548=CARTESIAN_POINT('Origin',(16.5633108984972,50.9766292734202,24.2));
#28549=CARTESIAN_POINT('Origin',(20.0789134070929,49.6970546047798,24.2));
#28550=CARTESIAN_POINT('Origin',(23.4966934678946,48.1753608816354,24.2));
#28551=CARTESIAN_POINT('Origin',(26.8,46.4189616428459,24.2));
#28552=CARTESIAN_POINT('Origin',(29.972739626032,44.4364138889502,24.2));
#28553=CARTESIAN_POINT('Origin',(32.9994550774553,42.2373763933203,11.));
#28554=CARTESIAN_POINT('Origin',(32.9994550774553,42.2373763933203,24.2));
#28555=CARTESIAN_POINT('Origin',(32.9994550774553,42.2373763933203,24.2));
#28556=CARTESIAN_POINT('Origin',(35.8654005008348,39.8325626455883,24.2));
#28557=CARTESIAN_POINT('Origin',(38.5566132981517,37.2336886566023,24.2));
#28558=CARTESIAN_POINT('Origin',(41.0599821511772,34.4534158791985,24.2));
#28559=CARTESIAN_POINT('Origin',(43.3633108984972,31.5052895228766,24.2));
#28560=CARTESIAN_POINT('Origin',(45.4553779539844,28.4036725628998,24.2));
#28561=CARTESIAN_POINT('Origin',(47.3259909772385,25.1636757653237,24.2));
#28562=CARTESIAN_POINT('Origin',(48.9660365296434,21.8010840688629,24.2));
#28563=CARTESIAN_POINT('Origin',(50.3675244741247,18.3322796822558,24.2));
#28564=CARTESIAN_POINT('Origin',(51.5236269022939,14.7741622717912,24.2));
#28565=CARTESIAN_POINT('Origin',(52.428711399332,11.1440666278319,11.));
#28566=CARTESIAN_POINT('Origin',(52.428711399332,11.1440666278319,24.2));
#28567=CARTESIAN_POINT('Origin',(52.428711399332,11.1440666278319,24.2));
#28568=CARTESIAN_POINT('Origin',(53.0783684845482,7.45967821145951,24.2));
#28569=CARTESIAN_POINT('Origin',(53.4694330939266,3.73894699268512,24.2));
#28570=CARTESIAN_POINT('Origin',(53.6,0.,24.2));
#28571=CARTESIAN_POINT('Origin',(-6.18033988749895,-19.0211303259031,14.5));
#28572=CARTESIAN_POINT('',(-7.68033988749895,-19.0211303259031,14.5));
#28573=CARTESIAN_POINT('Origin',(-6.18033988749895,-19.0211303259031,14.5));
#28574=CARTESIAN_POINT('',(-6.18033988749895,-19.0211303259031,16.));
#28575=CARTESIAN_POINT('',(-7.68033988749895,-19.0211303259031,14.5));
#28576=CARTESIAN_POINT('Origin',(-20.,2.44929359829471E-15,14.5));
#28577=CARTESIAN_POINT('',(-21.5,2.2655965784226E-15,14.5));
#28578=CARTESIAN_POINT('Origin',(-20.,2.44929359829471E-15,14.5));
#28579=CARTESIAN_POINT('',(-20.,2.44929359829471E-15,16.));
#28580=CARTESIAN_POINT('',(-21.5,2.2655965784226E-15,14.5));
#28581=CARTESIAN_POINT('Origin',(-6.18033988749895,19.0211303259031,14.5));
#28582=CARTESIAN_POINT('',(-7.68033988749895,19.0211303259031,14.5));
#28583=CARTESIAN_POINT('Origin',(-6.18033988749895,19.0211303259031,14.5));
#28584=CARTESIAN_POINT('',(-6.18033988749895,19.0211303259031,16.));
#28585=CARTESIAN_POINT('',(-7.68033988749895,19.0211303259031,14.5));
#28586=CARTESIAN_POINT('Origin',(16.1803398874989,11.7557050458495,14.5));
#28587=CARTESIAN_POINT('',(14.6803398874989,11.7557050458495,14.5));
#28588=CARTESIAN_POINT('Origin',(16.1803398874989,11.7557050458495,14.5));
#28589=CARTESIAN_POINT('',(16.1803398874989,11.7557050458495,16.));
#28590=CARTESIAN_POINT('',(14.6803398874989,11.7557050458495,14.5));
#28591=CARTESIAN_POINT('Origin',(16.1803398874989,-11.7557050458495,14.5));
#28592=CARTESIAN_POINT('',(14.6803398874989,-11.7557050458495,14.5));
#28593=CARTESIAN_POINT('Origin',(16.1803398874989,-11.7557050458495,14.5));
#28594=CARTESIAN_POINT('',(16.1803398874989,-11.7557050458495,16.));
#28595=CARTESIAN_POINT('',(14.6803398874989,-11.7557050458495,14.5));
#28596=CARTESIAN_POINT('Origin',(0.,0.,22.5));
#28597=CARTESIAN_POINT('',(-5.025,-6.15385016571545E-16,14.5));
#28598=CARTESIAN_POINT('',(-5.025,6.15385016571545E-16,22.5));
#28599=CARTESIAN_POINT('Origin',(0.,0.,14.5));
#28600=CARTESIAN_POINT('Origin',(0.,0.,14.5));
#28601=CARTESIAN_POINT('',(0.,0.,0.));
#28602=CARTESIAN_POINT('Origin',(-3.5,0.,0.));
#28603=CARTESIAN_POINT('',(-7.33651593783807,-9.64123956416204,0.000230242740474756));
#28604=CARTESIAN_POINT('',(-7.53848406216193,-9.64164981768271,-0.000239867588180398));
#28605=CARTESIAN_POINT('',(-3.5,-9.64155,-1.18074933463192E-15));
#28606=CARTESIAN_POINT('',(-8.,7.21801009705396,-6.39216838336781));
#28607=CARTESIAN_POINT('Ctrl Pts',(-7.53848406216193,-9.64164981768271,
-0.000239867588180398));
#28608=CARTESIAN_POINT('Ctrl Pts',(-7.55407606170334,-9.64036790708282,
1.25910592241467));
#28609=CARTESIAN_POINT('Ctrl Pts',(-7.56966806124475,-9.39229948530074,
2.51894068414412));
#28610=CARTESIAN_POINT('Ctrl Pts',(-7.58526006078616,-8.91143640847641,
3.6825791927546));
#28611=CARTESIAN_POINT('Ctrl Pts',(-7.6050095817011,-8.30235382302952,5.1564955433938));
#28612=CARTESIAN_POINT('Ctrl Pts',(-7.62475910261605,-7.31977820211336,
6.47607574498501));
#28613=CARTESIAN_POINT('Ctrl Pts',(-7.64450862353099,-6.08227773070946,
7.48205342360144));
#28614=CARTESIAN_POINT('Ctrl Pts',(-7.66425814444594,-4.84477725930556,
8.48803110221788));
#28615=CARTESIAN_POINT('Ctrl Pts',(-7.68400766536088,-3.35235193741391,
9.18040625785953));
#28616=CARTESIAN_POINT('Ctrl Pts',(-7.70375718627582,-1.78511818710048,
9.47566722361494));
#28617=CARTESIAN_POINT('Ctrl Pts',(-7.72350670719077,-0.21788443678705,
9.77092818937035));
#28618=CARTESIAN_POINT('Ctrl Pts',(-7.74325622810571,1.42415774194816,9.66907496523952));
#28619=CARTESIAN_POINT('Ctrl Pts',(-7.76300574902066,2.94287634303685,9.18231633088148));
#28620=CARTESIAN_POINT('Ctrl Pts',(-7.78275526993561,4.46159494412553,8.69555769652344));
#28621=CARTESIAN_POINT('Ctrl Pts',(-7.80250479085055,5.8569899675677,7.82389365193819));
#28622=CARTESIAN_POINT('Ctrl Pts',(-7.8222543117655,6.96061672529205,6.67267543875423));
#28623=CARTESIAN_POINT('Ctrl Pts',(-7.84200383268044,8.0642434830164,5.52145722557028));
#28624=CARTESIAN_POINT('Ctrl Pts',(-7.86175335359539,8.87610197502294,4.09068484378763));
#28625=CARTESIAN_POINT('Ctrl Pts',(-7.88150287451033,9.29832265436953,2.55270136385008));
#28626=CARTESIAN_POINT('Ctrl Pts',(-7.90125239542527,9.72054333371612,1.01471788391252));
#28627=CARTESIAN_POINT('Ctrl Pts',(-7.92100191634022,9.75312620040277,-0.630476694179928));
#28628=CARTESIAN_POINT('Ctrl Pts',(-7.94075143725517,9.39189406895472,-2.18363754482683));
#28629=CARTESIAN_POINT('Ctrl Pts',(-7.96050095817011,9.03066193750668,-3.73679839547375));
#28630=CARTESIAN_POINT('Ctrl Pts',(-7.98025047908506,8.27561480792393,-5.19792551867511));
#28631=CARTESIAN_POINT('Ctrl Pts',(-8.,7.21801009705396,-6.39216838336781));
#28632=CARTESIAN_POINT('',(-8.,-7.21857424983126,-6.39248700007983));
#28633=CARTESIAN_POINT('Origin',(-8.,0.,0.));
#28634=CARTESIAN_POINT('Ctrl Pts',(-8.,-7.21857424983126,-6.39248700007983));
#28635=CARTESIAN_POINT('Ctrl Pts',(-7.98217765815669,-6.26356488414857,
-7.46927134726881));
#28636=CARTESIAN_POINT('Ctrl Pts',(-7.96435531631337,-5.06448313044863,
-8.33050691837291));
#28637=CARTESIAN_POINT('Ctrl Pts',(-7.94653297447006,-3.73783082080585,
-8.88839335033359));
#28638=CARTESIAN_POINT('Ctrl Pts',(-7.92678345355512,-2.26772393101004,
-9.50660558377841));
#28639=CARTESIAN_POINT('Ctrl Pts',(-7.90703393264017,-0.640965728279816,
-9.75231774796247));
#28640=CARTESIAN_POINT('Ctrl Pts',(-7.88728441172523,0.946142179189394,
-9.59583455621896));
#28641=CARTESIAN_POINT('Ctrl Pts',(-7.86753489081029,2.53325008665859,-9.43935136447544));
#28642=CARTESIAN_POINT('Ctrl Pts',(-7.84778536989534,4.08070769886678,-8.88067281680435));
#28643=CARTESIAN_POINT('Ctrl Pts',(-7.82803584898039,5.40176465239776,-7.98724149155587));
#28644=CARTESIAN_POINT('Ctrl Pts',(-7.80828632806545,6.72282160592874,-7.09381016630739));
#28645=CARTESIAN_POINT('Ctrl Pts',(-7.7885368071505,7.81747790078251,-5.86562606348152));
#28646=CARTESIAN_POINT('Ctrl Pts',(-7.76878728623556,8.55363593826125,-4.4508923313193));
#28647=CARTESIAN_POINT('Ctrl Pts',(-7.74903776532061,9.28979397573999,-3.03615859915706));
#28648=CARTESIAN_POINT('Ctrl Pts',(-7.72928824440567,9.66745375584369,-1.43487523765846));
#28649=CARTESIAN_POINT('Ctrl Pts',(-7.70953872349072,9.64103836683124,0.159712143192118));
#28650=CARTESIAN_POINT('Ctrl Pts',(-7.68978920257578,9.61462297781878,1.75429952404268));
#28651=CARTESIAN_POINT('Ctrl Pts',(-7.67003968166083,9.18413241969018,3.34219092424522));
#28652=CARTESIAN_POINT('Ctrl Pts',(-7.65029016074589,8.40151829426746,4.73176596758706));
#28653=CARTESIAN_POINT('Ctrl Pts',(-7.63054063983094,7.61890416884475,6.1213410109289));
#28654=CARTESIAN_POINT('Ctrl Pts',(-7.61079111891599,6.48416647612792,7.31259969741003));
#28655=CARTESIAN_POINT('Ctrl Pts',(-7.59104159800105,5.13424258452846,8.16178175236003));
#28656=CARTESIAN_POINT('Ctrl Pts',(-7.57129207708611,3.78431869292901,9.01096380731002));
#28657=CARTESIAN_POINT('Ctrl Pts',(-7.55154255617117,2.21920860244693,9.51806923072888));
#28658=CARTESIAN_POINT('Ctrl Pts',(-7.53179303525622,0.627786835584183,
9.62190241167914));
#28659=CARTESIAN_POINT('Ctrl Pts',(-7.51204351434128,-0.963634931278574,
9.7257355926294));
#28660=CARTESIAN_POINT('Ctrl Pts',(-7.49229399342633,-2.581368374522,9.42629653111106));
#28661=CARTESIAN_POINT('Ctrl Pts',(-7.47254447251138,-4.03018885195262,
8.75972048847779));
#28662=CARTESIAN_POINT('Ctrl Pts',(-7.45279495159643,-5.47900932938324,
8.09314444584453));
#28663=CARTESIAN_POINT('Ctrl Pts',(-7.43304543068149,-6.75891684100106,
7.05943142209633));
#28664=CARTESIAN_POINT('Ctrl Pts',(-7.41329590976655,-7.71545470147883,
5.78332801562085));
#28665=CARTESIAN_POINT('Ctrl Pts',(-7.3935463888516,-8.67199256195661,4.50722460914537));
#28666=CARTESIAN_POINT('Ctrl Pts',(-7.37379686793666,-9.30516077129434,
2.9887308199426));
#28667=CARTESIAN_POINT('Ctrl Pts',(-7.35404734702171,-9.53854991728423,
1.41109525810262));
#28668=CARTESIAN_POINT('Ctrl Pts',(-7.3482035439605,-9.60760881808813,0.944279300112268));
#28669=CARTESIAN_POINT('Ctrl Pts',(-7.34235974089929,-9.64166529987996,
0.472285219261674));
#28670=CARTESIAN_POINT('Ctrl Pts',(-7.33651593783807,-9.64123956416204,
0.000230242740474756));
#28671=CARTESIAN_POINT('Origin',(-3.5,0.,0.));
#28672=CARTESIAN_POINT('',(-6.58651593783807,-9.64231270617946,-7.42785913304498E-5));
#28673=CARTESIAN_POINT('',(-6.78848406216194,-9.64077611273789,7.46528660069967E-5));
#28674=CARTESIAN_POINT('',(-3.5,-9.64155,-1.18074933463192E-15));
#28675=CARTESIAN_POINT('Ctrl Pts',(-6.78848406216194,-9.64077611273789,
7.46528660069967E-5));
#28676=CARTESIAN_POINT('Ctrl Pts',(-6.79733228980906,-9.64097151845064,
0.714921728157376));
#28677=CARTESIAN_POINT('Ctrl Pts',(-6.80618051745618,-9.56250642288335,
1.42972656374862));
#28678=CARTESIAN_POINT('Ctrl Pts',(-6.8150287451033,-9.40492023678117,2.12664053828175));
#28679=CARTESIAN_POINT('Ctrl Pts',(-6.83477826601825,-9.05318293949953,
3.68217433158735));
#28680=CARTESIAN_POINT('Ctrl Pts',(-6.85452778693319,-8.30726724506208,
5.14857650539751));
#28681=CARTESIAN_POINT('Ctrl Pts',(-6.87427730784814,-7.2571887358938,6.34888464751866));
#28682=CARTESIAN_POINT('Ctrl Pts',(-6.89402682876308,-6.20711022672555,
7.5491927896398));
#28683=CARTESIAN_POINT('Ctrl Pts',(-6.91377634967803,-4.85286890282648,
8.48340690007195));
#28684=CARTESIAN_POINT('Ctrl Pts',(-6.93352587059297,-3.35789183596898,
9.0387879216256));
#28685=CARTESIAN_POINT('Ctrl Pts',(-6.95327539150792,-1.86291476911148,
9.59416894317926));
#28686=CARTESIAN_POINT('Ctrl Pts',(-6.97302491242286,-0.227201959295531,
9.77071687585441));
#28687=CARTESIAN_POINT('Ctrl Pts',(-6.99277443333781,1.35185211055659,9.54712629195822));
#28688=CARTESIAN_POINT('Ctrl Pts',(-7.01252395425275,2.93090618040872,9.32353570806203));
#28689=CARTESIAN_POINT('Ctrl Pts',(-7.0322734751677,4.45330151029702,8.69980660759449));
#28690=CARTESIAN_POINT('Ctrl Pts',(-7.05202299608264,5.73531855391222,7.75120931257361));
#28691=CARTESIAN_POINT('Ctrl Pts',(-7.07177251699759,7.01733559752742,6.80261201755272));
#28692=CARTESIAN_POINT('Ctrl Pts',(-7.09152203791253,8.05897435486951,5.52914652797849));
#28693=CARTESIAN_POINT('Ctrl Pts',(-7.11127155882748,8.73453197137747,4.08449211495003));
#28694=CARTESIAN_POINT('Ctrl Pts',(-7.13102107974242,9.41008958788543,2.63983770192156));
#28695=CARTESIAN_POINT('Ctrl Pts',(-7.15077060065737,9.71956606355925,1.02399436543886));
#28696=CARTESIAN_POINT('Ctrl Pts',(-7.17052012157232,9.6256144463609,-0.568041338486824));
#28697=CARTESIAN_POINT('Ctrl Pts',(-7.19026964248726,9.53166282916255,-2.16007704241249));
#28698=CARTESIAN_POINT('Ctrl Pts',(-7.21001916340221,9.03428311909205,-3.72830511378114));
#28699=CARTESIAN_POINT('Ctrl Pts',(-7.22976868431715,8.19349801251508,-5.08347477399469));
#28700=CARTESIAN_POINT('Ctrl Pts',(-7.24951820523209,7.35271290593811,-6.43864443420824));
#28701=CARTESIAN_POINT('Ctrl Pts',(-7.26926772614704,6.16852240285469,-7.58075568326669));
#28702=CARTESIAN_POINT('Ctrl Pts',(-7.28901724706198,4.78383232783281,-8.37198129730586));
#28703=CARTESIAN_POINT('Ctrl Pts',(-7.30876676797693,3.39914225281091,-9.16320691134503));
#28704=CARTESIAN_POINT('Ctrl Pts',(-7.32851628889188,1.81395260585056,-9.60354689036491));
#28705=CARTESIAN_POINT('Ctrl Pts',(-7.34826580980682,0.219560570984832,
-9.63986108179457));
#28706=CARTESIAN_POINT('Ctrl Pts',(-7.36801533072177,-1.3748314638809,-9.67617527322422));
#28707=CARTESIAN_POINT('Ctrl Pts',(-7.38776485163671,-2.97842588665202,
-9.30846367706364));
#28708=CARTESIAN_POINT('Ctrl Pts',(-7.40751437255165,-4.39770369511272,
-8.58110256845882));
#28709=CARTESIAN_POINT('Ctrl Pts',(-7.4272638934666,-5.81698150357342,-7.85374145985401));
#28710=CARTESIAN_POINT('Ctrl Pts',(-7.44701341438155,-7.05194269772371,
-6.76673083880497));
#28711=CARTESIAN_POINT('Ctrl Pts',(-7.46676293529649,-7.95355566179962,
-5.45124585153094));
#28712=CARTESIAN_POINT('Ctrl Pts',(-7.48651245621144,-8.85516862587553,
-4.13576086425692));
#28713=CARTESIAN_POINT('Ctrl Pts',(-7.50626197712638,-9.42343335987706,
-2.59180151075793));
#28714=CARTESIAN_POINT('Ctrl Pts',(-7.52601149804132,-9.58977095188901,
-1.00569558416484));
#28715=CARTESIAN_POINT('Ctrl Pts',(-7.53016901941486,-9.62478709719151,
-0.671800432028954));
#28716=CARTESIAN_POINT('Ctrl Pts',(-7.5343265407884,-9.64199163213081,-0.336037532583489));
#28717=CARTESIAN_POINT('Ctrl Pts',(-7.53848406216193,-9.64164981768271,
-0.000239867588180398));
#28718=CARTESIAN_POINT('Ctrl Pts',(-7.33651593783807,-9.64123956416204,
0.000230242740474756));
#28719=CARTESIAN_POINT('Ctrl Pts',(-7.32261021998434,-9.64022649772028,
-1.12305595396952));
#28720=CARTESIAN_POINT('Ctrl Pts',(-7.30870450213061,-9.44396350863798,
-2.24668696246466));
#28721=CARTESIAN_POINT('Ctrl Pts',(-7.29479878427688,-9.05945974325286,
-3.30171374270337));
#28722=CARTESIAN_POINT('Ctrl Pts',(-7.27504926336193,-8.51337034058954,
-4.80010984719222));
#28723=CARTESIAN_POINT('Ctrl Pts',(-7.25529974244699,-7.58758145262085,
-6.16012472169274));
#28724=CARTESIAN_POINT('Ctrl Pts',(-7.23555022153204,-6.39381539850043,
-7.21763458266072));
#28725=CARTESIAN_POINT('Ctrl Pts',(-7.2158007006171,-5.20004934438002,-8.2751444436287));
#28726=CARTESIAN_POINT('Ctrl Pts',(-7.19605117970216,-3.73830612410787,
-9.03014929106414));
#28727=CARTESIAN_POINT('Ctrl Pts',(-7.17630165878721,-2.1849859165843,-9.39153666737156));
#28728=CARTESIAN_POINT('Ctrl Pts',(-7.15655213787226,-0.63166570906074,
-9.75292404367897));
#28729=CARTESIAN_POINT('Ctrl Pts',(-7.13680261695732,1.01323148571424,-9.72069394885837));
#28730=CARTESIAN_POINT('Ctrl Pts',(-7.11705309604237,2.55120283470161,-9.29873585321303));
#28731=CARTESIAN_POINT('Ctrl Pts',(-7.09730357512743,4.08917418368899,-8.8767777575677));
#28732=CARTESIAN_POINT('Ctrl Pts',(-7.07755405421249,5.52021968688874,-8.06509166109762));
#28733=CARTESIAN_POINT('Ctrl Pts',(-7.05780453329754,6.67164369979784,-6.96163017820614));
#28734=CARTESIAN_POINT('Ctrl Pts',(-7.03805501238259,7.82306771270693,-5.85816869531467));
#28735=CARTESIAN_POINT('Ctrl Pts',(-7.01830549146764,8.69487023532537,-4.46293182600177));
#28736=CARTESIAN_POINT('Ctrl Pts',(-6.9985559705527,9.18184392088289,-2.94429390550503));
#28737=CARTESIAN_POINT('Ctrl Pts',(-6.97880644963775,9.6688176064404,-1.42565598500829));
#28738=CARTESIAN_POINT('Ctrl Pts',(-6.95905692872282,9.77096245493699,0.216382986672299));
#28739=CARTESIAN_POINT('Ctrl Pts',(-6.93930740780787,9.47595183520748,1.78366510454321));
#28740=CARTESIAN_POINT('Ctrl Pts',(-6.91955788689293,9.18094121547797,3.35094722241412));
#28741=CARTESIAN_POINT('Ctrl Pts',(-6.89980836597798,8.48877512752234,4.84347248647533));
#28742=CARTESIAN_POINT('Ctrl Pts',(-6.88005884506304,7.48298275961571,6.08112599854471));
#28743=CARTESIAN_POINT('Ctrl Pts',(-6.86030932414809,6.47719039170906,7.3187795106141));
#28744=CARTESIAN_POINT('Ctrl Pts',(-6.84055980323314,5.15777174385139,8.30156127069164));
#28745=CARTESIAN_POINT('Ctrl Pts',(-6.8208102823182,3.68395156116386,8.91087118545994));
#28746=CARTESIAN_POINT('Ctrl Pts',(-6.80106076140325,2.21013137847635,9.52018110022824));
#28747=CARTESIAN_POINT('Ctrl Pts',(-6.78131124048831,0.58190966095899,9.7560191696873));
#28748=CARTESIAN_POINT('Ctrl Pts',(-6.76156171957337,-1.0042231232646,9.58992493759571));
#28749=CARTESIAN_POINT('Ctrl Pts',(-6.74181219865842,-2.59035590748818,
9.42383070550413));
#28750=CARTESIAN_POINT('Ctrl Pts',(-6.72206267774348,-4.13439975841799,
8.85580417186189));
#28751=CARTESIAN_POINT('Ctrl Pts',(-6.70231315682853,-5.45002262070945,
7.95439361757151));
#28752=CARTESIAN_POINT('Ctrl Pts',(-6.68256363591358,-6.76564548300091,
7.05298306328113));
#28753=CARTESIAN_POINT('Ctrl Pts',(-6.66281411499864,-7.85284735665405,
5.81818848834261));
#28754=CARTESIAN_POINT('Ctrl Pts',(-6.64306459408369,-8.58042694222024,
4.39902237762939));
#28755=CARTESIAN_POINT('Ctrl Pts',(-6.62421504200182,-9.27485134628063,
3.04452645684594));
#28756=CARTESIAN_POINT('Ctrl Pts',(-6.60536548991995,-9.64168205182771,
1.52207945153344));
#28757=CARTESIAN_POINT('Ctrl Pts',(-6.58651593783807,-9.64231270617946,
-7.42785913304498E-5));
#28758=CARTESIAN_POINT('Origin',(-3.5,0.,0.));
#28759=CARTESIAN_POINT('',(-5.83651593783807,-9.6409035792506,-0.000152919944957977));
#28760=CARTESIAN_POINT('',(-6.03848406216193,-9.6421289025524,0.00016016297285322));
#28761=CARTESIAN_POINT('',(-3.5,-9.64155,-1.18074933463192E-15));
#28762=CARTESIAN_POINT('Ctrl Pts',(-6.03848406216193,-9.6421289025524,0.00016016297285322));
#28763=CARTESIAN_POINT('Ctrl Pts',(-6.04058851791477,-9.6422628445658,0.170110221396648));
#28764=CARTESIAN_POINT('Ctrl Pts',(-6.04269297366761,-9.63786113934538,
0.340053343096354));
#28765=CARTESIAN_POINT('Ctrl Pts',(-6.04479742942045,-9.62887717318408,
0.509753879367992));
#28766=CARTESIAN_POINT('Ctrl Pts',(-6.0645469503354,-9.54456605029038,2.10232919764383));
#28767=CARTESIAN_POINT('Ctrl Pts',(-6.08429647125035,-9.05669006237452,
3.67353974494806));
#28768=CARTESIAN_POINT('Ctrl Pts',(-6.10404599216529,-8.22412508625499,
5.03377504457948));
#28769=CARTESIAN_POINT('Ctrl Pts',(-6.12379551308023,-7.39156011013546,
6.3940103442109));
#28770=CARTESIAN_POINT('Ctrl Pts',(-6.14354503399518,-6.21430614581225,
7.54327039616953));
#28771=CARTESIAN_POINT('Ctrl Pts',(-6.16329455491012,-4.83443179494827,
8.34286484690855));
#28772=CARTESIAN_POINT('Ctrl Pts',(-6.18304407582506,-3.45455744408426,
9.14245929764759));
#28773=CARTESIAN_POINT('Ctrl Pts',(-6.20279359674001,-1.87206270667947,
9.59238814716702));
#28774=CARTESIAN_POINT('Ctrl Pts',(-6.22254311765496,-0.277919812425482,
9.63835490172843));
#28775=CARTESIAN_POINT('Ctrl Pts',(-6.2422926385699,1.3162230818285,9.68432165628985));
#28776=CARTESIAN_POINT('Ctrl Pts',(-6.26204215948485,2.92201413293167,9.32632631589325));
#28777=CARTESIAN_POINT('Ctrl Pts',(-6.28179168039979,4.34566975967897,8.6075710263458));
#28778=CARTESIAN_POINT('Ctrl Pts',(-6.30154120131473,5.76932538642627,7.88881573679835));
#28779=CARTESIAN_POINT('Ctrl Pts',(-6.32129072222968,7.01084558881768,6.80930049810006));
#28780=CARTESIAN_POINT('Ctrl Pts',(-6.34104024314462,7.92040624696886,5.49929900230839));
#28781=CARTESIAN_POINT('Ctrl Pts',(-6.36078976405957,8.82996690512002,4.18929750651673));
#28782=CARTESIAN_POINT('Ctrl Pts',(-6.38053928497452,9.40756801903096,2.6488097536317));
#28783=CARTESIAN_POINT('Ctrl Pts',(-6.40028880588946,9.5835058671029,1.06373865635419));
#28784=CARTESIAN_POINT('Ctrl Pts',(-6.42003832680441,9.75944371517485,-0.521332440923332));
#28785=CARTESIAN_POINT('Ctrl Pts',(-6.43978784771935,9.53371829740781,-2.15098688259333));
#28786=CARTESIAN_POINT('Ctrl Pts',(-6.45953736863429,8.93356969576332,-3.62856130230734));
#28787=CARTESIAN_POINT('Ctrl Pts',(-6.47928688954924,8.33342109411885,-5.10613572202132));
#28788=CARTESIAN_POINT('Ctrl Pts',(-6.49903641046419,7.35884930859695,-6.43163011977932));
#28789=CARTESIAN_POINT('Ctrl Pts',(-6.51878593137913,6.12746366985518,-7.44508654138933));
#28790=CARTESIAN_POINT('Ctrl Pts',(-6.53853545229408,4.89607803111339,-8.45854296299935));
#28791=CARTESIAN_POINT('Ctrl Pts',(-6.55828497320902,3.40787853915171,-9.15996140846138));
#28792=CARTESIAN_POINT('Ctrl Pts',(-6.57803449412397,1.84245806626817,-9.4646961339002));
#28793=CARTESIAN_POINT('Ctrl Pts',(-6.59778401503891,0.277037593384629,
-9.76943085933902));
#28794=CARTESIAN_POINT('Ctrl Pts',(-6.61753353595386,-1.36560386042078,
-9.67748186475465));
#28795=CARTESIAN_POINT('Ctrl Pts',(-6.6372830568688,-2.88723568278026,-9.19994536652855));
#28796=CARTESIAN_POINT('Ctrl Pts',(-6.65703257778374,-4.40886750513973,
-8.72240886830246));
#28797=CARTESIAN_POINT('Ctrl Pts',(-6.67678209869869,-5.80948969605326,
-7.85928486643466));
#28798=CARTESIAN_POINT('Ctrl Pts',(-6.69653161961364,-6.92007803273464,
-6.7147334015106));
#28799=CARTESIAN_POINT('Ctrl Pts',(-6.71628114052858,-8.03066636941602,
-5.57018193658653));
#28800=CARTESIAN_POINT('Ctrl Pts',(-6.73603066144353,-8.85122085186524,
-4.14420300860619));
#28801=CARTESIAN_POINT('Ctrl Pts',(-6.75578018235847,-9.28271864302694,
-2.6088808382155));
#28802=CARTESIAN_POINT('Ctrl Pts',(-6.7666814756263,-9.52089576064561,-1.7614173826664));
#28803=CARTESIAN_POINT('Ctrl Pts',(-6.77758276889412,-9.64053536678673,
-0.880639307056883));
#28804=CARTESIAN_POINT('Ctrl Pts',(-6.78848406216194,-9.64077611273789,
7.46528660069967E-5));
#28805=CARTESIAN_POINT('Ctrl Pts',(-6.58651593783807,-9.64231270617946,
-7.42785913304498E-5));
#28806=CARTESIAN_POINT('Ctrl Pts',(-6.585615969005,-9.64234281667007,-0.0727492636680994));
#28807=CARTESIAN_POINT('Ctrl Pts',(-6.58471600017193,-9.64153814863087,
-0.145423580203645));
#28808=CARTESIAN_POINT('Ctrl Pts',(-6.58381603133886,-9.63989450023572,
-0.218078916870951));
#28809=CARTESIAN_POINT('Ctrl Pts',(-6.56406651042392,-9.60382517520572,
-1.81247645417013));
#28810=CARTESIAN_POINT('Ctrl Pts',(-6.54431698950897,-9.16372922766646,
-3.39773388228055));
#28811=CARTESIAN_POINT('Ctrl Pts',(-6.52456746859402,-8.37271653684779,
-4.78254557565492));
#28812=CARTESIAN_POINT('Ctrl Pts',(-6.50481794767908,-7.58170384602911,
-6.16735726902929));
#28813=CARTESIAN_POINT('Ctrl Pts',(-6.48506842676413,-6.43977441193101,
-7.3517232276676));
#28814=CARTESIAN_POINT('Ctrl Pts',(-6.46531890584919,-5.08473394412332,
-8.19271658896709));
#28815=CARTESIAN_POINT('Ctrl Pts',(-6.44556938493425,-3.72969347631562,
-9.03370995026658));
#28816=CARTESIAN_POINT('Ctrl Pts',(-6.4258198640193,-2.16154197479832,-9.53133071422725));
#28817=CARTESIAN_POINT('Ctrl Pts',(-6.40607034310436,-0.569520756880948,
-9.6255270243824));
#28818=CARTESIAN_POINT('Ctrl Pts',(-6.38632082218941,1.02250046103641,-9.71972333453754));
#28819=CARTESIAN_POINT('Ctrl Pts',(-6.36657130127447,2.63839139535383,-9.41049519088718));
#28820=CARTESIAN_POINT('Ctrl Pts',(-6.34682178035952,4.08314963161027,-8.73515961362618));
#28821=CARTESIAN_POINT('Ctrl Pts',(-6.32707225944458,5.52790786786671,-8.05982403636518));
#28822=CARTESIAN_POINT('Ctrl Pts',(-6.30732273852963,6.80153340606216,-7.01838102549355));
#28823=CARTESIAN_POINT('Ctrl Pts',(-6.28757321761468,7.75032772001901,-5.73650979446092));
#28824=CARTESIAN_POINT('Ctrl Pts',(-6.26782369669974,8.69912203397587,-4.45463856342828));
#28825=CARTESIAN_POINT('Ctrl Pts',(-6.2480741757848,9.32308512369412,-2.93233911223461));
#28826=CARTESIAN_POINT('Ctrl Pts',(-6.22832465486985,9.54691839912312,-1.35331942649404));
#28827=CARTESIAN_POINT('Ctrl Pts',(-6.20857513395491,9.77075167455211,0.225700259246526));
#28828=CARTESIAN_POINT('Ctrl Pts',(-6.18882561303996,9.59445513569186,1.86144017953401));
#28829=CARTESIAN_POINT('Ctrl Pts',(-6.16907609212501,9.03930388843518,3.35650258485865));
#28830=CARTESIAN_POINT('Ctrl Pts',(-6.14932657121007,8.48415264117849,4.8515649901833));
#28831=CARTESIAN_POINT('Ctrl Pts',(-6.12957705029513,7.55014668552537,6.2059498805451));
#28832=CARTESIAN_POINT('Ctrl Pts',(-6.10982752938018,6.34999995074282,7.25621285624999));
#28833=CARTESIAN_POINT('Ctrl Pts',(-6.09007800846524,5.14985321596029,8.30647583195487));
#28834=CARTESIAN_POINT('Ctrl Pts',(-6.07032848755029,3.68356570204834,9.05261689300285));
#28835=CARTESIAN_POINT('Ctrl Pts',(-6.05057896663535,2.12808598853988,9.40459326154099));
#28836=CARTESIAN_POINT('Ctrl Pts',(-6.0308294457204,0.572606275031421,9.75656963007913));
#28837=CARTESIAN_POINT('Ctrl Pts',(-6.01107992480545,-1.07206563807355,
9.71438130610743));
#28838=CARTESIAN_POINT('Ctrl Pts',(-5.99133040389051,-2.60745410663262,
9.28311949031393));
#28839=CARTESIAN_POINT('Ctrl Pts',(-5.97158088297557,-4.1428425751917,8.85185767452044));
#28840=CARTESIAN_POINT('Ctrl Pts',(-5.95183136206062,-5.5689475992049,8.03152236690513));
#28841=CARTESIAN_POINT('Ctrl Pts',(-5.93208184114568,-6.71366973987204,
6.92110995531557));
#28842=CARTESIAN_POINT('Ctrl Pts',(-5.91233232023073,-7.85839188053918,
5.810697543726));
#28843=CARTESIAN_POINT('Ctrl Pts',(-5.89258279931578,-8.72173113786027,
4.41020802816217));
#28844=CARTESIAN_POINT('Ctrl Pts',(-5.87283327840084,-9.19950149525361,
2.88864962023233));
#28845=CARTESIAN_POINT('Ctrl Pts',(-5.86072749821325,-9.49235836766379,
1.9559864073723));
#28846=CARTESIAN_POINT('Ctrl Pts',(-5.84862171802566,-9.64034658300698,
0.977834339335062));
#28847=CARTESIAN_POINT('Ctrl Pts',(-5.83651593783807,-9.6409035792506,-0.000152919944957977));
#28848=CARTESIAN_POINT('Origin',(-3.5,0.,0.));
#28849=CARTESIAN_POINT('',(-5.08651593783807,-9.64135114576405,0.000239874805416028));
#28850=CARTESIAN_POINT('',(-5.28848406216194,-9.64152836430215,-0.000244200588832011));
#28851=CARTESIAN_POINT('',(-3.5,-9.64155,-1.18074933463192E-15));
#28852=CARTESIAN_POINT('Ctrl Pts',(-5.28848406216194,-9.64152836430215,
-0.000244200588832011));
#28853=CARTESIAN_POINT('Ctrl Pts',(-5.30359426693543,-9.64029754505796,
1.2202338220874));
#28854=CARTESIAN_POINT('Ctrl Pts',(-5.31870447170893,-9.40769088764861,
2.44116766783866));
#28855=CARTESIAN_POINT('Ctrl Pts',(-5.33381467648243,-8.95537463172337,
3.57440762075094));
#28856=CARTESIAN_POINT('Ctrl Pts',(-5.35356419739738,-8.36418281860958,
5.0555884840934));
#28857=CARTESIAN_POINT('Ctrl Pts',(-5.37331371831232,-7.39765393457124,
6.38695901098043));
#28858=CARTESIAN_POINT('Ctrl Pts',(-5.39306323922727,-6.17242670938371,
7.40785212805192));
#28859=CARTESIAN_POINT('Ctrl Pts',(-5.41281276014221,-4.94719948419616,
8.42874524512343));
#28860=CARTESIAN_POINT('Ctrl Pts',(-5.43256228105716,-3.46327391785939,
9.1391609523794));
#28861=CARTESIAN_POINT('Ctrl Pts',(-5.4523118019721,-1.89972711401413,9.45336773462645));
#28862=CARTESIAN_POINT('Ctrl Pts',(-5.47206132288705,-0.336180310168875,
9.76757451687349));
#28863=CARTESIAN_POINT('Ctrl Pts',(-5.49181084380199,1.30698773118489,9.6855723741116));
#28864=CARTESIAN_POINT('Ctrl Pts',(-5.51156036471694,2.83148285007319,9.2172571572859));
#28865=CARTESIAN_POINT('Ctrl Pts',(-5.53130988563188,4.35597796896149,8.74894194046021));
#28866=CARTESIAN_POINT('Ctrl Pts',(-5.55105940654683,5.76180016538431,7.89431364957073));
#28867=CARTESIAN_POINT('Ctrl Pts',(-5.57080892746177,6.8792976907094,6.7565070795787));
#28868=CARTESIAN_POINT('Ctrl Pts',(-5.59055844837672,7.99679521603447,5.61870050958668));
#28869=CARTESIAN_POINT('Ctrl Pts',(-5.61030796929166,8.8259680702618,4.1977156604921));
#28870=CARTESIAN_POINT('Ctrl Pts',(-5.6300574902066,9.26675336848597,2.66503407885353));
#28871=CARTESIAN_POINT('Ctrl Pts',(-5.64980701112155,9.70753866671014,1.13235249721493));
#28872=CARTESIAN_POINT('Ctrl Pts',(-5.6695565320365,9.75993640893116,-0.512025816967684));
#28873=CARTESIAN_POINT('Ctrl Pts',(-5.68930605295145,9.41762334273858,-2.06966065046962));
#28874=CARTESIAN_POINT('Ctrl Pts',(-5.70905557386639,9.07531027654599,-3.62729548397154));
#28875=CARTESIAN_POINT('Ctrl Pts',(-5.72880509478133,8.33828640193982,-5.09818683679275));
#28876=CARTESIAN_POINT('Ctrl Pts',(-5.74855461569628,7.29549425335211,-6.30483054753282));
#28877=CARTESIAN_POINT('Ctrl Pts',(-5.76830413661122,6.2527021047644,-7.51147425827288));
#28878=CARTESIAN_POINT('Ctrl Pts',(-5.78805365752617,4.90414168219518,-8.45387032693178));
#28879=CARTESIAN_POINT('Ctrl Pts',(-5.80780317844112,3.41255450047279,-9.01829232255752));
#28880=CARTESIAN_POINT('Ctrl Pts',(-5.82755269935606,1.92096731875038,-9.58271431818327));
#28881=CARTESIAN_POINT('Ctrl Pts',(-5.847302220271,0.286353377874808,-9.76916224077585));
#28882=CARTESIAN_POINT('Ctrl Pts',(-5.86705174118594,-1.29402545353786,
-9.5551359362069));
#28883=CARTESIAN_POINT('Ctrl Pts',(-5.88680126210089,-2.87440428495053,
-9.34110963163796));
#28884=CARTESIAN_POINT('Ctrl Pts',(-5.90655078301584,-4.4005480069003,-8.72660909990748));
#28885=CARTESIAN_POINT('Ctrl Pts',(-5.92630030393079,-5.68828471503698,
-7.78579100891321));
#28886=CARTESIAN_POINT('Ctrl Pts',(-5.94604982484573,-6.97602142317366,
-6.84497291791894));
#28887=CARTESIAN_POINT('Ctrl Pts',(-5.96579934576067,-8.02535111749725,
-5.57783726766087));
#28888=CARTESIAN_POINT('Ctrl Pts',(-5.98554886667561,-8.70964283572328,
-4.1372993979081));
#28889=CARTESIAN_POINT('Ctrl Pts',(-6.00319393183772,-9.32101827161303,
-2.85026136342924));
#28890=CARTESIAN_POINT('Ctrl Pts',(-6.02083899699983,-9.64100584945367,
-1.42480676785808));
#28891=CARTESIAN_POINT('Ctrl Pts',(-6.03848406216193,-9.6421289025524,0.00016016297285322));
#28892=CARTESIAN_POINT('Ctrl Pts',(-5.83651593783807,-9.6409035792506,-0.000152919944957977));
#28893=CARTESIAN_POINT('Ctrl Pts',(-5.82887219711071,-9.64125527363182,
-0.6176662837061));
#28894=CARTESIAN_POINT('Ctrl Pts',(-5.82122845638336,-9.58282883544997,
-1.23511394122783));
#28895=CARTESIAN_POINT('Ctrl Pts',(-5.81358471565601,-9.46497918425804,
-1.84100337620655));
#28896=CARTESIAN_POINT('Ctrl Pts',(-5.79383519474106,-9.16048505840356,
-3.4064706644198));
#28897=CARTESIAN_POINT('Ctrl Pts',(-5.77408567382611,-8.459295349229,-4.89477794055051));
#28898=CARTESIAN_POINT('Ctrl Pts',(-5.75433615291117,-7.44602819734076,
-6.12631932517789));
#28899=CARTESIAN_POINT('Ctrl Pts',(-5.73458663199622,-6.43276104545249,
-7.35786070980529));
#28900=CARTESIAN_POINT('Ctrl Pts',(-5.71483711108128,-5.10741645085051,
-8.33263620292937));
#28901=CARTESIAN_POINT('Ctrl Pts',(-5.69508759016634,-3.62993428970603,
-8.93301189084948));
#28902=CARTESIAN_POINT('Ctrl Pts',(-5.67533806925139,-2.15245212856156,
-9.53338757876959));
#28903=CARTESIAN_POINT('Ctrl Pts',(-5.65558854833645,-0.522832400874613,
-9.75936346148576));
#28904=CARTESIAN_POINT('Ctrl Pts',(-5.6358390274215,1.06226571617635,-9.58366923145192));
#28905=CARTESIAN_POINT('Ctrl Pts',(-5.61608950650656,2.6473638332273,-9.40797500141808));
#28906=CARTESIAN_POINT('Ctrl Pts',(-5.59633998559161,4.18794033964224,-8.83061065863424));
#28907=CARTESIAN_POINT('Ctrl Pts',(-5.57659046467667,5.49808161214777,-7.92125135163658));
#28908=CARTESIAN_POINT('Ctrl Pts',(-5.55684094376172,6.80822288465331,-7.01189204463891));
#28909=CARTESIAN_POINT('Ctrl Pts',(-5.53709142284678,7.88792892324943,-5.77053777342741));
#28910=CARTESIAN_POINT('Ctrl Pts',(-5.51734190193183,8.60690301052564,-4.3469926336545));
#28911=CARTESIAN_POINT('Ctrl Pts',(-5.49759238101689,9.32587709780184,-2.92344749388162));
#28912=CARTESIAN_POINT('Ctrl Pts',(-5.47784286010194,9.68411923375813,-1.31771148554732));
#28913=CARTESIAN_POINT('Ctrl Pts',(-5.458093339187,9.63839748980967,0.276438452593999));
#28914=CARTESIAN_POINT('Ctrl Pts',(-5.43834381827205,9.5926757458612,1.87058839073534));
#28915=CARTESIAN_POINT('Ctrl Pts',(-5.41859429735711,9.14299012200796,3.4531522586837));
#28916=CARTESIAN_POINT('Ctrl Pts',(-5.39884477644216,8.34360776000916,4.83314948421386));
#28917=CARTESIAN_POINT('Ctrl Pts',(-5.37909525552722,7.54422539801037,6.21314670974401));
#28918=CARTESIAN_POINT('Ctrl Pts',(-5.35934573461227,6.39514629786602,7.39057729285595));
#28919=CARTESIAN_POINT('Ctrl Pts',(-5.33959621369733,5.03503897622948,8.22335131789296));
#28920=CARTESIAN_POINT('Ctrl Pts',(-5.31984669278238,3.67493165459292,9.05612534292997));
#28921=CARTESIAN_POINT('Ctrl Pts',(-5.30009717186744,2.10379611146416,9.54424280989203));
#28922=CARTESIAN_POINT('Ctrl Pts',(-5.28034765095249,0.511233772193015,
9.62879870076278));
#28923=CARTESIAN_POINT('Ctrl Pts',(-5.26059813003755,-1.08132856707812,
9.71335459163353));
#28924=CARTESIAN_POINT('Ctrl Pts',(-5.24084860912261,-2.69531770249161,
9.39434890641299));
#28925=CARTESIAN_POINT('Ctrl Pts',(-5.22109908820766,-4.13596072478972,
8.71027859902533));
#28926=CARTESIAN_POINT('Ctrl Pts',(-5.20134956729271,-5.57660374708781,
8.02620829163769));
#28927=CARTESIAN_POINT('Ctrl Pts',(-5.18160004637777,-6.8439006562705,6.97707336208295));
#28928=CARTESIAN_POINT('Ctrl Pts',(-5.16185052546282,-7.78491665217157,
5.68948126883141));
#28929=CARTESIAN_POINT('Ctrl Pts',(-5.14210100454788,-8.72593264807268,
4.40188917557982));
#28930=CARTESIAN_POINT('Ctrl Pts',(-5.12235148363294,-9.34066773069216,
2.87583991863138));
#28931=CARTESIAN_POINT('Ctrl Pts',(-5.10260196271799,-9.55493692701037,
1.2954940024931));
#28932=CARTESIAN_POINT('Ctrl Pts',(-5.09723995442469,-9.61311115881104,
0.866429016809633));
#28933=CARTESIAN_POINT('Ctrl Pts',(-5.09187794613138,-9.64176600192921,
0.433361682257971));
#28934=CARTESIAN_POINT('Ctrl Pts',(-5.08651593783807,-9.64135114576405,
0.000239874805416028));
#28935=CARTESIAN_POINT('Origin',(-3.5,0.,0.));
#28936=CARTESIAN_POINT('',(-4.33651593783807,-9.64225279696581,-0.000111202327370922));
#28937=CARTESIAN_POINT('',(-4.53848406216194,-9.64081637547245,0.000107710467356636));
#28938=CARTESIAN_POINT('',(-3.5,-9.64155,-1.18074933463192E-15));
#28939=CARTESIAN_POINT('Ctrl Pts',(-4.53848406216194,-9.64081637547245,
0.000107710467356636));
#28940=CARTESIAN_POINT('Ctrl Pts',(-4.54685049504115,-9.64108436120108,
0.676022573073167));
#28941=CARTESIAN_POINT('Ctrl Pts',(-4.55521692792037,-9.57099666503678,
1.35188265298491));
#28942=CARTESIAN_POINT('Ctrl Pts',(-4.56358336079958,-9.42998123846142,
2.01260489815126));
#28943=CARTESIAN_POINT('Ctrl Pts',(-4.58333288171452,-9.09710495095793,
3.57228367502892));
#28944=CARTESIAN_POINT('Ctrl Pts',(-4.60308240262947,-8.36899991173037,
5.04761028815404));
#28945=CARTESIAN_POINT('Ctrl Pts',(-4.62283192354442,-7.33353234839077,
6.26054533797998));
#28946=CARTESIAN_POINT('Ctrl Pts',(-4.64258144445936,-6.29806478505116,
7.47348038780594));
#28947=CARTESIAN_POINT('Ctrl Pts',(-4.6623309653743,-4.95523469759951,8.42402387433271));
#28948=CARTESIAN_POINT('Ctrl Pts',(-4.68208048628925,-3.46709207573716,
8.99746615287645));
#28949=CARTESIAN_POINT('Ctrl Pts',(-4.70183000720419,-1.97894945387482,
9.57090843142019));
#28950=CARTESIAN_POINT('Ctrl Pts',(-4.72157952811914,-0.345494297601781,
9.7672495019809));
#28951=CARTESIAN_POINT('Ctrl Pts',(-4.74132904903409,1.23615136422273,9.56279532555869));
#28952=CARTESIAN_POINT('Ctrl Pts',(-4.76107856994903,2.81779702604719,9.35834114913648));
#28953=CARTESIAN_POINT('Ctrl Pts',(-4.78082809086397,4.34763319342313,8.75309172573136));
#28954=CARTESIAN_POINT('Ctrl Pts',(-4.80057761177892,5.64104236523506,7.82008731840125));
#28955=CARTESIAN_POINT('Ctrl Pts',(-4.82032713269386,6.93445153704702,6.88708291107111));
#28956=CARTESIAN_POINT('Ctrl Pts',(-4.84007665360881,7.99143371329496,5.62632351981596));
#28957=CARTESIAN_POINT('Ctrl Pts',(-4.85982617452376,8.6844344458204,4.18995501050368));
#28958=CARTESIAN_POINT('Ctrl Pts',(-4.8795756954387,9.37743517834584,2.75358650119141));
#28959=CARTESIAN_POINT('Ctrl Pts',(-4.89932521635364,9.70645446714877,1.141608873822));
#28960=CARTESIAN_POINT('Ctrl Pts',(-4.91907473726859,9.63178693709627,-0.451447707025219));
#28961=CARTESIAN_POINT('Ctrl Pts',(-4.93882425818353,9.55711940704377,-2.04450428787242));
#28962=CARTESIAN_POINT('Ctrl Pts',(-4.95857377909848,9.07876505813585,-3.61863982219743));
#28963=CARTESIAN_POINT('Ctrl Pts',(-4.97832330001343,8.25445071526159,-4.98389085184599));
#28964=CARTESIAN_POINT('Ctrl Pts',(-4.99807282092837,7.43013637238733,-6.34914188149456));
#28965=CARTESIAN_POINT('Ctrl Pts',(-5.01782234184331,6.25986203554674,-7.50550840646669));
#28966=CARTESIAN_POINT('Ctrl Pts',(-5.03757186275826,4.8848540192266,-8.31344247857905));
#28967=CARTESIAN_POINT('Ctrl Pts',(-5.0573213836732,3.50984600290644,-9.12137655069141));
#28968=CARTESIAN_POINT('Ctrl Pts',(-5.07707090458815,1.93010430710673,-9.580878169944));
#28969=CARTESIAN_POINT('Ctrl Pts',(-5.0968204255031,0.336268930087386,-9.63649562032042));
#28970=CARTESIAN_POINT('Ctrl Pts',(-5.11656994641804,-1.25756644693194,
-9.69211307069684));
#28971=CARTESIAN_POINT('Ctrl Pts',(-5.13631946733298,-2.86549550517089,
-9.34384635219709));
#28972=CARTESIAN_POINT('Ctrl Pts',(-5.15606898824793,-4.29347665309604,
-8.63372358042091));
#28973=CARTESIAN_POINT('Ctrl Pts',(-5.17581850916287,-5.72145780102118,
-7.92360080864472));
#28974=CARTESIAN_POINT('Ctrl Pts',(-5.19556803007782,-6.96949103863252,
-6.8516219835921));
#28975=CARTESIAN_POINT('Ctrl Pts',(-5.21531755099276,-7.88696626626681,
-5.54715131834045));
#28976=CARTESIAN_POINT('Ctrl Pts',(-5.23506707190771,-8.80444149390112,
-4.24268065308877));
#28977=CARTESIAN_POINT('Ctrl Pts',(-5.25481659282265,-9.39135871155838,
-2.70571814763806));
#28978=CARTESIAN_POINT('Ctrl Pts',(-5.2745661137376,-9.57688994929239,-1.12174129501374));
#28979=CARTESIAN_POINT('Ctrl Pts',(-5.27920542987904,-9.62047268072516,
-0.749652806806595));
#28980=CARTESIAN_POINT('Ctrl Pts',(-5.28384474602049,-9.64190626517592,
-0.374969988608132));
#28981=CARTESIAN_POINT('Ctrl Pts',(-5.28848406216194,-9.64152836430215,
-0.000244200588832011));
#28982=CARTESIAN_POINT('Ctrl Pts',(-5.08651593783807,-9.64135114576405,
0.000239874805416028));
#28983=CARTESIAN_POINT('Ctrl Pts',(-5.07212842521643,-9.64023799039654,
-1.16192644992957));
#28984=CARTESIAN_POINT('Ctrl Pts',(-5.05774091259479,-9.42983072252804,
-2.32448496508033));
#28985=CARTESIAN_POINT('Ctrl Pts',(-5.04335339997315,-9.01881669295193,
-3.41116839932792));
#28986=CARTESIAN_POINT('Ctrl Pts',(-5.02360387905821,-8.45462395255836,
-4.90284230968261));
#28987=CARTESIAN_POINT('Ctrl Pts',(-5.00385435814326,-7.51243516175428,
-6.2515475550639));
#28988=CARTESIAN_POINT('Ctrl Pts',(-4.98410483722832,-6.30595173762386,
-7.29452514372254));
#28989=CARTESIAN_POINT('Ctrl Pts',(-4.96435531631337,-5.09946831349343,
-8.3375027323812));
#28990=CARTESIAN_POINT('Ctrl Pts',(-4.94460579539843,-3.62869025603665,
-9.0747526643172));
#28991=CARTESIAN_POINT('Ctrl Pts',(-4.92485627448348,-2.07110805440109,
-9.41730512496206));
#28992=CARTESIAN_POINT('Ctrl Pts',(-4.90510675356854,-0.513525852765532,
-9.75985758560692));
#28993=CARTESIAN_POINT('Ctrl Pts',(-4.88535723265359,1.13086049304882,-9.70771257496064));
#28994=CARTESIAN_POINT('Ctrl Pts',(-4.86560771173865,2.66360980057637,-9.26716284630389));
#28995=CARTESIAN_POINT('Ctrl Pts',(-4.8458581908237,4.19635910810388,-8.82661311764716));
#28996=CARTESIAN_POINT('Ctrl Pts',(-4.82610866990876,5.61747137734461,-7.99765867097999));
#28997=CARTESIAN_POINT('Ctrl Pts',(-4.80635914899381,6.75544968493727,-6.88033603422992));
#28998=CARTESIAN_POINT('Ctrl Pts',(-4.78660962807887,7.89342799252996,-5.76301339747983));
#28999=CARTESIAN_POINT('Ctrl Pts',(-4.76686010716393,8.74827233847458,-4.35732257064681));
#29000=CARTESIAN_POINT('Ctrl Pts',(-4.74711058624898,9.2168218547275,-2.83289944894966));
#29001=CARTESIAN_POINT('Ctrl Pts',(-4.72736106533404,9.68537137098043,-1.3084763272525));
#29002=CARTESIAN_POINT('Ctrl Pts',(-4.70761154441909,9.76762605754167,0.334679089308759));
#29003=CARTESIAN_POINT('Ctrl Pts',(-4.68786202350414,9.45365958699668,1.89827416429438));
#29004=CARTESIAN_POINT('Ctrl Pts',(-4.6681125025892,9.1396931164517,3.46186923927994));
#29005=CARTESIAN_POINT('Ctrl Pts',(-4.64836298167426,8.42950548880053,4.94590397268984));
#29006=CARTESIAN_POINT('Ctrl Pts',(-4.62861346075931,7.40880069505612,6.17128808682416));
#29007=CARTESIAN_POINT('Ctrl Pts',(-4.60886393984437,6.38809590131167,7.39667220095852));
#29008=CARTESIAN_POINT('Ctrl Pts',(-4.58911441892942,5.05687394147397,8.36340569581729));
#29009=CARTESIAN_POINT('Ctrl Pts',(-4.56936489801448,3.57578396013533,8.95482514960961));
#29010=CARTESIAN_POINT('Ctrl Pts',(-4.54961537709953,2.09469397879668,9.54624460340193));
#29011=CARTESIAN_POINT('Ctrl Pts',(-4.52986585618459,0.463735975957077,
9.76235001612781));
#29012=CARTESIAN_POINT('Ctrl Pts',(-4.51011633526964,-1.12026937089548,
9.57706222838065));
#29013=CARTESIAN_POINT('Ctrl Pts',(-4.4903668143547,-2.70427471774801,9.39177444063348));
#29014=CARTESIAN_POINT('Ctrl Pts',(-4.47061729343975,-4.24132740861351,
8.80509345241328));
#29015=CARTESIAN_POINT('Ctrl Pts',(-4.45086777252481,-5.54593906707505,
7.88781872598075));
#29016=CARTESIAN_POINT('Ctrl Pts',(-4.43111825160986,-6.85055072553659,
6.97054399954821));
#29017=CARTESIAN_POINT('Ctrl Pts',(-4.41136873069492,-7.92272135159418,
5.72267553490333));
#29018=CARTESIAN_POINT('Ctrl Pts',(-4.39161920977997,-8.63306358601724,
4.2948035472446));
#29019=CARTESIAN_POINT('Ctrl Pts',(-4.373251452466,-9.29370714430582,2.96683178237609));
#29020=CARTESIAN_POINT('Ctrl Pts',(-4.35488369515204,-9.64138137487533,
1.48316305483911));
#29021=CARTESIAN_POINT('Ctrl Pts',(-4.33651593783807,-9.64225279696581,
-0.000111202327370922));
#29022=CARTESIAN_POINT('Origin',(-3.5,0.,0.));
#29023=CARTESIAN_POINT('',(-3.58651593783807,-9.64084195522704,-0.000123447406648672));
#29024=CARTESIAN_POINT('',(-3.78848406216194,-9.64221558294609,0.000128484054292971));
#29025=CARTESIAN_POINT('',(-3.5,-9.64155,-1.18074933463192E-15));
#29026=CARTESIAN_POINT('Ctrl Pts',(-3.78848406216194,-9.64221558294609,
0.000128484054292971));
#29027=CARTESIAN_POINT('Ctrl Pts',(-3.79010672314687,-9.64230233742042,
0.131166705674271));
#29028=CARTESIAN_POINT('Ctrl Pts',(-3.7917293841318,-9.63968591491053,0.262201459667352));
#29029=CARTESIAN_POINT('Ctrl Pts',(-3.79335204511673,-9.63434364026827,
0.393124986510688));
#29030=CARTESIAN_POINT('Ctrl Pts',(-3.81310156603167,-9.56932244005419,
1.98660443518506));
#29031=CARTESIAN_POINT('Ctrl Pts',(-3.83285108694662,-9.10050726460994,
3.56360725535284));
#29032=CARTESIAN_POINT('Ctrl Pts',(-3.85260060786156,-8.28447377087269,
4.93382397066609));
#29033=CARTESIAN_POINT('Ctrl Pts',(-3.87235012877651,-7.46844027713545,
6.30404068597931));
#29034=CARTESIAN_POINT('Ctrl Pts',(-3.89209964969145,-6.30518846510522,
7.46747129643801));
#29035=CARTESIAN_POINT('Ctrl Pts',(-3.9118491706064,-4.93509718533139,8.28371537446398));
#29036=CARTESIAN_POINT('Ctrl Pts',(-3.93159869152134,-3.56500590555757,
9.09995945248994));
#29037=CARTESIAN_POINT('Ctrl Pts',(-3.95134821243629,-1.98807515804016,
9.56901699808319));
#29038=CARTESIAN_POINT('Ctrl Pts',(-3.97109773335123,-0.394605721546979,
9.63428310557247));
#29039=CARTESIAN_POINT('Ctrl Pts',(-3.99084725426618,1.1988637149462,9.69954921306175));
#29040=CARTESIAN_POINT('Ctrl Pts',(-4.01059677518112,2.80887184041515,9.36102388244707));
#29041=CARTESIAN_POINT('Ctrl Pts',(-4.03034629609607,4.24112616574349,8.65955965855324));
#29042=CARTESIAN_POINT('Ctrl Pts',(-4.05009581701101,5.67338049107185,7.95809543465941));
#29043=CARTESIAN_POINT('Ctrl Pts',(-4.06984533792595,6.92788101625959,6.89369231748643));
#29044=CARTESIAN_POINT('Ctrl Pts',(-4.0895948588409,7.85323718260037,5.59480029917241));
#29045=CARTESIAN_POINT('Ctrl Pts',(-4.10934437975584,8.77859334894114,4.29590828085841));
#29046=CARTESIAN_POINT('Ctrl Pts',(-4.12909390067079,9.37480515643494,2.76252736140337));
#29047=CARTESIAN_POINT('Ctrl Pts',(-4.14884342158574,9.56992298303575,1.17970281535688));
#29048=CARTESIAN_POINT('Ctrl Pts',(-4.16859294250068,9.76504080963655,-0.403121730689601));
#29049=CARTESIAN_POINT('Ctrl Pts',(-4.18834246341562,9.55906465534435,-2.03538990332756));
#29050=CARTESIAN_POINT('Ctrl Pts',(-4.20809198433057,8.97685130136602,-3.52012291645618));
#29051=CARTESIAN_POINT('Ctrl Pts',(-4.22784150524551,8.39463794738768,-5.00485592958482));
#29052=CARTESIAN_POINT('Ctrl Pts',(-4.24759102616046,7.43618739372319,-6.34205378320413));
#29053=CARTESIAN_POINT('Ctrl Pts',(-4.26734054707541,6.21716349375353,-7.37034617407725));
#29054=CARTESIAN_POINT('Ctrl Pts',(-4.28709006799035,4.99813959378387,-8.39863856495036));
#29055=CARTESIAN_POINT('Ctrl Pts',(-4.30683958890529,3.51854234750906,-9.11802549307728));
#29056=CARTESIAN_POINT('Ctrl Pts',(-4.32658910982024,1.95692652575344,-9.44169281467044));
#29057=CARTESIAN_POINT('Ctrl Pts',(-4.34633863073518,0.395310703997839,
-9.7653601362636));
#29058=CARTESIAN_POINT('Ctrl Pts',(-4.36608815165013,-1.24832369323855,
-9.69330785132303));
#29059=CARTESIAN_POINT('Ctrl Pts',(-4.38583767256508,-2.7756262271073,-9.23423108229325));
#29060=CARTESIAN_POINT('Ctrl Pts',(-4.40558719348002,-4.30292876097604,
-8.77515431326348));
#29061=CARTESIAN_POINT('Ctrl Pts',(-4.42533671439496,-5.71389943147713,
-7.9290530601445));
#29062=CARTESIAN_POINT('Ctrl Pts',(-4.44508623530991,-6.83826518265192,
-6.7980330924119));
#29063=CARTESIAN_POINT('Ctrl Pts',(-4.46483575622485,-7.96263093382673,
-5.66701312467929));
#29064=CARTESIAN_POINT('Ctrl Pts',(-4.4845852771398,-8.80039176567523,-4.25107444233305));
#29065=CARTESIAN_POINT('Ctrl Pts',(-4.50433479805475,-9.25044841370977,
-2.72108963084481));
#29066=CARTESIAN_POINT('Ctrl Pts',(-4.51571788609048,-9.50984885525497,
-1.83924789516393));
#29067=CARTESIAN_POINT('Ctrl Pts',(-4.52710097412621,-9.64045176307607,
-0.919519387099601));
#29068=CARTESIAN_POINT('Ctrl Pts',(-4.53848406216194,-9.64081637547245,
0.000107710467356636));
#29069=CARTESIAN_POINT('Ctrl Pts',(-4.33651593783807,-9.64225279696581,
-0.000111202327370922));
#29070=CARTESIAN_POINT('Ctrl Pts',(-4.33513417423709,-9.64231835201998,
-0.111694469886249));
#29071=CARTESIAN_POINT('Ctrl Pts',(-4.33375241063611,-9.64042127976813,
-0.223275505057436));
#29072=CARTESIAN_POINT('Ctrl Pts',(-4.33237064703514,-9.63654717632921,
-0.334787855250616));
#29073=CARTESIAN_POINT('Ctrl Pts',(-4.31262112612019,-9.58117468942955,
-1.92863175941445));
#29074=CARTESIAN_POINT('Ctrl Pts',(-4.29287160520524,-9.12191587284169,
-3.50844405706951));
#29075=CARTESIAN_POINT('Ctrl Pts',(-4.2731220842903,-8.31419314165281,-4.88357622986835));
#29076=CARTESIAN_POINT('Ctrl Pts',(-4.25337256337535,-7.50647041046394,
-6.25870840266719));
#29077=CARTESIAN_POINT('Ctrl Pts',(-4.23362304246041,-6.35028376467405,
-7.42916045060979));
#29078=CARTESIAN_POINT('Ctrl Pts',(-4.21387352154547,-4.98515944501452,
-8.25368461339688));
#29079=CARTESIAN_POINT('Ctrl Pts',(-4.19412400063052,-3.62003512535496,
-9.07820877618398));
#29080=CARTESIAN_POINT('Ctrl Pts',(-4.17437447971558,-2.04597313182576,
-9.55680505381556));
#29081=CARTESIAN_POINT('Ctrl Pts',(-4.15462495880063,-0.452928047828257,
-9.63171742593875));
#29082=CARTESIAN_POINT('Ctrl Pts',(-4.13487543788569,1.14011703616925,-9.70662979806195));
#29083=CARTESIAN_POINT('Ctrl Pts',(-4.11512591697074,2.75214521063503,-9.37785826467676));
#29084=CARTESIAN_POINT('Ctrl Pts',(-4.0953763960558,4.18862021106955,-8.6850783022988));
#29085=CARTESIAN_POINT('Ctrl Pts',(-4.07562687514085,5.62509521150404,-7.99229833992086));
#29086=CARTESIAN_POINT('Ctrl Pts',(-4.05587735422591,6.88601703790726,-6.93550994855018));
#29087=CARTESIAN_POINT('Ctrl Pts',(-4.03612783331096,7.81922022206973,-5.64224419078239));
#29088=CARTESIAN_POINT('Ctrl Pts',(-4.01637831239602,8.75242340623219,-4.34897843301462));
#29089=CARTESIAN_POINT('Ctrl Pts',(-3.99662879148107,9.35790794815393,-2.8192353088497));
#29090=CARTESIAN_POINT('Ctrl Pts',(-3.97687927056613,9.56260521115508,-1.23762109113875));
#29091=CARTESIAN_POINT('Ctrl Pts',(-3.95712974965118,9.76730247415624,0.343993126572243));
#29092=CARTESIAN_POINT('Ctrl Pts',(-3.93738022873624,9.57121245823682,1.97747843782926));
#29093=CARTESIAN_POINT('Ctrl Pts',(-3.91763070782129,8.99799890563587,3.46570917473141));
#29094=CARTESIAN_POINT('Ctrl Pts',(-3.89788118690635,8.42478535303492,4.95393991163352));
#29095=CARTESIAN_POINT('Ctrl Pts',(-3.8781316659914,7.47444826375242,6.29691607418075));
#29096=CARTESIAN_POINT('Ctrl Pts',(-3.85838214507646,6.26167237487477,7.33257004462774));
#29097=CARTESIAN_POINT('Ctrl Pts',(-3.83863262416151,5.04889648599708,8.36822401507476));
#29098=CARTESIAN_POINT('Ctrl Pts',(-3.81888310324657,3.57368179752421,9.09655579342157));
#29099=CARTESIAN_POINT('Ctrl Pts',(-3.79913358233162,2.01405420216457,9.42967178964279));
#29100=CARTESIAN_POINT('Ctrl Pts',(-3.77938406141668,0.454426606804935,
9.762787785864));
#29101=CARTESIAN_POINT('Ctrl Pts',(-3.75963454050173,-1.18961389544146,
9.7006879999596));
#29102=CARTESIAN_POINT('Ctrl Pts',(-3.73988501958679,-2.71966785780379,
9.25086650713709));
#29103=CARTESIAN_POINT('Ctrl Pts',(-3.72013549867184,-4.2497218201661,8.80104501431459));
#29104=CARTESIAN_POINT('Ctrl Pts',(-3.7003859777569,-5.66578924264433,7.96350181457399));
#29105=CARTESIAN_POINT('Ctrl Pts',(-3.68063645684195,-6.79698200367094,
6.83930990900508));
#29106=CARTESIAN_POINT('Ctrl Pts',(-3.66088693592701,-7.92817476469756,
5.71511800343617));
#29107=CARTESIAN_POINT('Ctrl Pts',(-3.64113741501206,-8.77449286427254,
4.30427739203897));
#29108=CARTESIAN_POINT('Ctrl Pts',(-3.62138789409712,-9.23380436433331,
2.77704543550532));
#29109=CARTESIAN_POINT('Ctrl Pts',(-3.60976390867744,-9.50414156404529,
1.87816175768467));
#29110=CARTESIAN_POINT('Ctrl Pts',(-3.59813992325775,-9.64041378177036,
0.938958344725818));
#29111=CARTESIAN_POINT('Ctrl Pts',(-3.58651593783807,-9.64084195522704,
-0.000123447406648672));
#29112=CARTESIAN_POINT('Origin',(-3.5,0.,0.));
#29113=CARTESIAN_POINT('',(-2.83651593783807,-9.64146833476739,0.000244149912687573));
#29114=CARTESIAN_POINT('',(-3.03848406216193,-9.6414091844932,-0.000242700028759701));
#29115=CARTESIAN_POINT('',(-3.5,-9.64155,-1.18074933463192E-15));
#29116=CARTESIAN_POINT('Ctrl Pts',(-3.03848406216193,-9.6414091844932,-0.000242700028759701));
#29117=CARTESIAN_POINT('Ctrl Pts',(-3.05311247216753,-9.64025195196911,
1.18136192116153));
#29118=CARTESIAN_POINT('Ctrl Pts',(-3.06774088217312,-9.42257645101838,
2.36338120258475));
#29119=CARTESIAN_POINT('Ctrl Pts',(-3.08236929217871,-8.99799891745031,
3.46570917928206));
#29120=CARTESIAN_POINT('Ctrl Pts',(-3.10211881309366,-8.42478536409669,
4.95393991813827));
#29121=CARTESIAN_POINT('Ctrl Pts',(-3.1218683340086,-7.47444827356636,6.2969160824488));
#29122=CARTESIAN_POINT('Ctrl Pts',(-3.14161785492354,-6.26167238309626,
7.33257005425562));
#29123=CARTESIAN_POINT('Ctrl Pts',(-3.16136737583849,-5.0488964926262,8.36822402606241));
#29124=CARTESIAN_POINT('Ctrl Pts',(-3.18111689675343,-3.57368180221639,
9.0965558053655));
#29125=CARTESIAN_POINT('Ctrl Pts',(-3.20086641766838,-2.01405420480899,
9.42967180202408));
#29126=CARTESIAN_POINT('Ctrl Pts',(-3.22061593858332,-0.45442660740154,
9.76278779868267));
#29127=CARTESIAN_POINT('Ctrl Pts',(-3.24036545949827,1.1896138970035,9.70068801269671));
#29128=CARTESIAN_POINT('Ctrl Pts',(-3.26011498041321,2.71966786137481,9.25086651928357));
#29129=CARTESIAN_POINT('Ctrl Pts',(-3.27986450132816,4.24972182574611,8.80104502587043));
#29130=CARTESIAN_POINT('Ctrl Pts',(-3.2996140222431,5.66578925008368,7.9635018250301));
#29131=CARTESIAN_POINT('Ctrl Pts',(-3.31936354315805,6.79698201259557,6.83930991798508));
#29132=CARTESIAN_POINT('Ctrl Pts',(-3.33911306407299,7.92817477510741,5.7151180109401));
#29133=CARTESIAN_POINT('Ctrl Pts',(-3.35886258498794,8.77449287579359,4.30427739769045));
#29134=CARTESIAN_POINT('Ctrl Pts',(-3.37861210590288,9.23380437645742,2.77704543915155));
#29135=CARTESIAN_POINT('Ctrl Pts',(-3.39836162681783,9.69311587712127,1.24981348061261));
#29136=CARTESIAN_POINT('Ctrl Pts',(-3.41811114773277,9.76542077776275,-0.393809823215587));
#29137=CARTESIAN_POINT('Ctrl Pts',(-3.43786066864772,9.44199347079099,-1.9554753722144));
#29138=CARTESIAN_POINT('Ctrl Pts',(-3.45761018956266,9.11856616381923,-3.51714092121322));
#29139=CARTESIAN_POINT('Ctrl Pts',(-3.47735971047761,8.39940664923424,-4.99684871538265));
#29140=CARTESIAN_POINT('Ctrl Pts',(-3.49710923139255,7.37130162702222,-6.21603064320442));
#29141=CARTESIAN_POINT('Ctrl Pts',(-3.5168587523075,6.3431966048102,-7.43521257102619));
#29142=CARTESIAN_POINT('Ctrl Pts',(-3.53660827322244,5.00614607497117,-8.39386863250029));
#29143=CARTESIAN_POINT('Ctrl Pts',(-3.55635779413739,3.52150256200938,-8.97631017398341));
#29144=CARTESIAN_POINT('Ctrl Pts',(-3.57610731505233,2.03685904904759,-9.55875171546654));
#29145=CARTESIAN_POINT('Ctrl Pts',(-3.59585683596728,0.404622552963038,
-9.76497873695868));
#29146=CARTESIAN_POINT('Ctrl Pts',(-3.61560635688222,-1.1782319628052,-9.57010418311216));
#29147=CARTESIAN_POINT('Ctrl Pts',(-3.63535587779717,-2.76108647857339,
-9.37522962926565));
#29148=CARTESIAN_POINT('Ctrl Pts',(-3.65510539871212,-4.29455901402527,
-8.7792535000805));
#29149=CARTESIAN_POINT('Ctrl Pts',(-3.67485491962706,-5.59359323858005,
-7.85409697642628));
#29150=CARTESIAN_POINT('Ctrl Pts',(-3.694604440542,-6.89262746313484,-6.92894045277205));
#29151=CARTESIAN_POINT('Ctrl Pts',(-3.71435396145695,-7.95722337679252,
-5.67460353464874));
#29152=CARTESIAN_POINT('Ctrl Pts',(-3.73410348237189,-8.6589077211294,-4.24245703699665));
#29153=CARTESIAN_POINT('Ctrl Pts',(-3.7522303423019,-9.30294024625533,-2.92797862134267));
#29154=CARTESIAN_POINT('Ctrl Pts',(-3.77035720223192,-9.64124644261487,
-1.4637087011892));
#29155=CARTESIAN_POINT('Ctrl Pts',(-3.78848406216194,-9.64221558294609,
0.000128484054292971));
#29156=CARTESIAN_POINT('Ctrl Pts',(-3.58651593783807,-9.64084195522704,
-0.000123447406648672));
#29157=CARTESIAN_POINT('Ctrl Pts',(-3.57839040234281,-9.6411412620908,-0.656571486476391));
#29158=CARTESIAN_POINT('Ctrl Pts',(-3.57026486684754,-9.57506099308481,
-1.31296009608115));
#29159=CARTESIAN_POINT('Ctrl Pts',(-3.56213933135228,-9.44199345839355,
-1.95547536964678));
#29160=CARTESIAN_POINT('Ctrl Pts',(-3.54238981043734,-9.11856615184647,
-3.51714091659511));
#29161=CARTESIAN_POINT('Ctrl Pts',(-3.52264028952239,-8.39940663820575,
-4.99684870882167));
#29162=CARTESIAN_POINT('Ctrl Pts',(-3.50289076860745,-7.37130161734365,
-6.21603063504264));
#29163=CARTESIAN_POINT('Ctrl Pts',(-3.4831412476925,-6.34319659648157,-7.4352125612636));
#29164=CARTESIAN_POINT('Ctrl Pts',(-3.46339172677756,-5.00614606839814,
-8.39386862147897));
#29165=CARTESIAN_POINT('Ctrl Pts',(-3.44364220586261,-3.52150255738573,
-8.97631016219736));
#29166=CARTESIAN_POINT('Ctrl Pts',(-3.42389268494767,-2.03685904637332,
-9.55875170291574));
#29167=CARTESIAN_POINT('Ctrl Pts',(-3.40414316403272,-0.404622552431944,
-9.76497872413714));
#29168=CARTESIAN_POINT('Ctrl Pts',(-3.38439364311778,1.17823196125796,-9.57010417054653));
#29169=CARTESIAN_POINT('Ctrl Pts',(-3.36464412220284,2.76108647494785,-9.37522961695592));
#29170=CARTESIAN_POINT('Ctrl Pts',(-3.34489460128789,4.29455900838627,-8.77925348855332));
#29171=CARTESIAN_POINT('Ctrl Pts',(-3.32514508037294,5.59359323123543,-7.85409696611386));
#29172=CARTESIAN_POINT('Ctrl Pts',(-3.305395559458,6.89262745408462,-6.92894044367438));
#29173=CARTESIAN_POINT('Ctrl Pts',(-3.28564603854305,7.95722336634453,-5.67460352719801));
#29174=CARTESIAN_POINT('Ctrl Pts',(-3.26589651762811,8.65890770976012,-4.24245703142631));
#29175=CARTESIAN_POINT('Ctrl Pts',(-3.24614699671316,9.36059205317571,-2.81031053565461));
#29176=CARTESIAN_POINT('Ctrl Pts',(-3.22639747579822,9.69936482774697,-1.20035446058757));
#29177=CARTESIAN_POINT('Ctrl Pts',(-3.20664795488328,9.63434362761826,0.393124985994513));
#29178=CARTESIAN_POINT('Ctrl Pts',(-3.18689843396833,9.56932242748955,1.9866044325766));
#29179=CARTESIAN_POINT('Ctrl Pts',(-3.16714891305338,9.10050725266087,3.56360725067374));
#29180=CARTESIAN_POINT('Ctrl Pts',(-3.14739939213844,8.28447375999511,4.93382396418786));
#29181=CARTESIAN_POINT('Ctrl Pts',(-3.12764987122349,7.46844026732935,6.30404067770196));
#29182=CARTESIAN_POINT('Ctrl Pts',(-3.10790035030855,6.30518845682652,7.46747128663305));
#29183=CARTESIAN_POINT('Ctrl Pts',(-3.0881508293936,4.93509717885166,8.28371536358729));
#29184=CARTESIAN_POINT('Ctrl Pts',(-3.06840130847866,3.56500590087681,9.09995944054153));
#29185=CARTESIAN_POINT('Ctrl Pts',(-3.04865178756371,1.98807515542992,9.56901698551892));
#29186=CARTESIAN_POINT('Ctrl Pts',(-3.02890226664877,0.39460572102899,9.63428309292253));
#29187=CARTESIAN_POINT('Ctrl Pts',(-3.00915274573382,-1.19886371337197,
9.69954920032614));
#29188=CARTESIAN_POINT('Ctrl Pts',(-2.98940322481888,-2.80887183672698,
9.36102387015595));
#29189=CARTESIAN_POINT('Ctrl Pts',(-2.96965370390394,-4.24112616017478,
8.65955964718316));
#29190=CARTESIAN_POINT('Ctrl Pts',(-2.94990418298899,-5.67338048362257,
7.95809542421037));
#29191=CARTESIAN_POINT('Ctrl Pts',(-2.93015466207404,-6.92788100716316,
6.89369230843497));
#29192=CARTESIAN_POINT('Ctrl Pts',(-2.9104051411591,-7.85323717228894,5.59480029182642));
#29193=CARTESIAN_POINT('Ctrl Pts',(-2.89065562024415,-8.77859333741471,
4.29590827521789));
#29194=CARTESIAN_POINT('Ctrl Pts',(-2.87090609932921,-9.37480514412569,
2.7625273577762));
#29195=CARTESIAN_POINT('Ctrl Pts',(-2.85115657841426,-9.56992297047031,
1.17970281380798));
#29196=CARTESIAN_POINT('Ctrl Pts',(-2.84627636488886,-9.61813764156408,
0.78857830091096));
#29197=CARTESIAN_POINT('Ctrl Pts',(-2.84139615136346,-9.64186107894428,
0.394434706521363));
#29198=CARTESIAN_POINT('Ctrl Pts',(-2.83651593783807,-9.64146833476739,
0.000244149912687573));
#29199=CARTESIAN_POINT('Origin',(-3.5,0.,0.));
#29200=CARTESIAN_POINT('',(-2.08651593783807,-9.64217411726438,-0.000144835560233357));
#29201=CARTESIAN_POINT('',(-2.28848406216193,-9.64087107694564,0.000138544266770069));
#29202=CARTESIAN_POINT('',(-3.5,-9.64155,-1.18074933463192E-15));
#29203=CARTESIAN_POINT('Ctrl Pts',(-2.28848406216193,-9.64087107694564,
0.000138544266770069));
#29204=CARTESIAN_POINT('Ctrl Pts',(-2.29636870027324,-9.64119830166034,
0.637119391179249));
#29205=CARTESIAN_POINT('Ctrl Pts',(-2.30425333838455,-9.57900501984992,
1.27403718462593));
#29206=CARTESIAN_POINT('Ctrl Pts',(-2.31213797649586,-9.45365959940943,
1.89827416678697));
#29207=CARTESIAN_POINT('Ctrl Pts',(-2.3318874974108,-9.13969312845218,3.46186924382557));
#29208=CARTESIAN_POINT('Ctrl Pts',(-2.35163701832575,-8.42950549986849,
4.94590397918403));
#29209=CARTESIAN_POINT('Ctrl Pts',(-2.37138653924069,-7.40880070478383,
6.17128809492729));
#29210=CARTESIAN_POINT('Ctrl Pts',(-2.39113606015564,-6.38809590969918,
7.39667221067056));
#29211=CARTESIAN_POINT('Ctrl Pts',(-2.41088558107058,-5.05687394811357,
8.36340570679862));
#29212=CARTESIAN_POINT('Ctrl Pts',(-2.43063510198553,-3.57578396483025,
8.95482516136745));
#29213=CARTESIAN_POINT('Ctrl Pts',(-2.45038462290047,-2.09469398154692,
9.54624461593629));
#29214=CARTESIAN_POINT('Ctrl Pts',(-2.47013414381541,-0.463735976565879,
9.76235002894589));
#29215=CARTESIAN_POINT('Ctrl Pts',(-2.48988366473036,1.12026937236647,9.57706224095543));
#29216=CARTESIAN_POINT('Ctrl Pts',(-2.50963318564531,2.7042747212988,9.39177445296498));
#29217=CARTESIAN_POINT('Ctrl Pts',(-2.52938270656025,4.24132741418244,8.80509346397447));
#29218=CARTESIAN_POINT('Ctrl Pts',(-2.54913222747519,5.54593907435693,7.88781873633755));
#29219=CARTESIAN_POINT('Ctrl Pts',(-2.56888174839014,6.85055073453146,6.97054400870061));
#29220=CARTESIAN_POINT('Ctrl Pts',(-2.58863126930509,7.92272136199684,5.72267554241725));
#29221=CARTESIAN_POINT('Ctrl Pts',(-2.60838079022003,8.63306359735259,4.29480355288367));
#29222=CARTESIAN_POINT('Ctrl Pts',(-2.62813031113498,9.34340583270835,2.8669315633501));
#29223=CARTESIAN_POINT('Ctrl Pts',(-2.64787983204992,9.6919196759545,1.25905605056633));
#29224=CARTESIAN_POINT('Ctrl Pts',(-2.66762935296487,9.63654718898212,-0.334787855690263));
#29225=CARTESIAN_POINT('Ctrl Pts',(-2.68737887387981,9.58117470200974,-1.92863176194685));
#29226=CARTESIAN_POINT('Ctrl Pts',(-2.70712839479476,9.12191588481883,-3.50844406167626));
#29227=CARTESIAN_POINT('Ctrl Pts',(-2.7268779157097,8.31419315256938,-4.88357623628066));
#29228=CARTESIAN_POINT('Ctrl Pts',(-2.74662743662464,7.50647042031993,-6.25870841088505));
#29229=CARTESIAN_POINT('Ctrl Pts',(-2.76637695753959,6.35028377301195,-7.42916046036445));
#29230=CARTESIAN_POINT('Ctrl Pts',(-2.78612647845453,4.98515945155998,-8.25368462423414));
#29231=CARTESIAN_POINT('Ctrl Pts',(-2.80587599936948,3.62003513010801,-9.07820878810382));
#29232=CARTESIAN_POINT('Ctrl Pts',(-2.82562552028443,2.04597313451206,-9.55680506636378));
#29233=CARTESIAN_POINT('Ctrl Pts',(-2.84537504119937,0.452928048422888,
-9.63171743858532));
#29234=CARTESIAN_POINT('Ctrl Pts',(-2.86512456211431,-1.1401170376663,-9.70662981080687));
#29235=CARTESIAN_POINT('Ctrl Pts',(-2.88487408302926,-2.7521452142487,-9.37785827698998));
#29236=CARTESIAN_POINT('Ctrl Pts',(-2.9046236039442,-4.18862021656932,-8.68507831370239));
#29237=CARTESIAN_POINT('Ctrl Pts',(-2.92437312485915,-5.62509521888996,
-7.99229835041479));
#29238=CARTESIAN_POINT('Ctrl Pts',(-2.9441226457741,-6.8860170469488,-6.93550995765648));
#29239=CARTESIAN_POINT('Ctrl Pts',(-2.96387216668904,-7.81922023233658,
-5.64224419819056));
#29240=CARTESIAN_POINT('Ctrl Pts',(-2.98362168760399,-8.75242341772432,
-4.3489784387247));
#29241=CARTESIAN_POINT('Ctrl Pts',(-3.00337120851893,-9.35790796044102,
-2.81923531255126));
#29242=CARTESIAN_POINT('Ctrl Pts',(-3.02312072943387,-9.56260522371092,
-1.23762109276363));
#29243=CARTESIAN_POINT('Ctrl Pts',(-3.02824184034323,-9.61568384736771,
-0.827503709652114));
#29244=CARTESIAN_POINT('Ctrl Pts',(-3.03336295125258,-9.64181430822856,
-0.413898614363083));
#29245=CARTESIAN_POINT('Ctrl Pts',(-3.03848406216193,-9.6414091844932,-0.000242700028759701));
#29246=CARTESIAN_POINT('Ctrl Pts',(-2.83651593783807,-9.64146833476739,
0.000244149912687573));
#29247=CARTESIAN_POINT('Ctrl Pts',(-2.82164663044852,-9.64027169985349,
-1.20079767454136));
#29248=CARTESIAN_POINT('Ctrl Pts',(-2.80677732305897,-9.41519657160002,
-2.40227546481473));
#29249=CARTESIAN_POINT('Ctrl Pts',(-2.79190801566943,-8.9768512895793,-3.52012291183421));
#29250=CARTESIAN_POINT('Ctrl Pts',(-2.77215849475448,-8.39463793636543,
-5.00485592301334));
#29251=CARTESIAN_POINT('Ctrl Pts',(-2.75240897383954,-7.43618738395943,
-6.34205377487687));
#29252=CARTESIAN_POINT('Ctrl Pts',(-2.7326594529246,-6.21716348559042,-7.37034616439981));
#29253=CARTESIAN_POINT('Ctrl Pts',(-2.71290993200965,-4.99813958722139,
-8.39863855392276));
#29254=CARTESIAN_POINT('Ctrl Pts',(-2.6931604110947,-3.51854234288933,-9.11802548110512));
#29255=CARTESIAN_POINT('Ctrl Pts',(-2.67341089017976,-1.95692652318417,
-9.44169280227334));
#29256=CARTESIAN_POINT('Ctrl Pts',(-2.65366136926481,-0.395310703478979,
-9.76536012344156));
#29257=CARTESIAN_POINT('Ctrl Pts',(-2.63391184834987,1.24832369159934,-9.69330783859562));
#29258=CARTESIAN_POINT('Ctrl Pts',(-2.61416232743493,2.77562622346274,-9.23423107016863));
#29259=CARTESIAN_POINT('Ctrl Pts',(-2.59441280651998,4.30292875532614,-8.77515430174165));
#29260=CARTESIAN_POINT('Ctrl Pts',(-2.57466328560503,5.71389942397464,-7.92905304973361));
#29261=CARTESIAN_POINT('Ctrl Pts',(-2.55491376469009,6.83826517367314,-6.79803308348605));
#29262=CARTESIAN_POINT('Ctrl Pts',(-2.53516424377514,7.96263092337165,-5.66701311723849));
#29263=CARTESIAN_POINT('Ctrl Pts',(-2.5154147228602,8.80039175412018,-4.25107443675139));
#29264=CARTESIAN_POINT('Ctrl Pts',(-2.49566520194525,9.2504484015638,-2.72108962727205));
#29265=CARTESIAN_POINT('Ctrl Pts',(-2.47591568103031,9.70050504900742,-1.19110481779274));
#29266=CARTESIAN_POINT('Ctrl Pts',(-2.45616616011537,9.76285751314615,0.452926120678768));
#29267=CARTESIAN_POINT('Ctrl Pts',(-2.43641663920042,9.42998122607976,2.01260489550855));
#29268=CARTESIAN_POINT('Ctrl Pts',(-2.41666711828548,9.09710493901337,3.57228367033836));
#29269=CARTESIAN_POINT('Ctrl Pts',(-2.39691759737053,8.36899990074182,5.04761028152639));
#29270=CARTESIAN_POINT('Ctrl Pts',(-2.37716807645558,7.3335323387618,6.26054532975976));
#29271=CARTESIAN_POINT('Ctrl Pts',(-2.35741855554064,6.29806477678178,7.47348037799312));
#29272=CARTESIAN_POINT('Ctrl Pts',(-2.3376690346257,4.95523469109328,8.42402386327183));
#29273=CARTESIAN_POINT('Ctrl Pts',(-2.31791951371075,3.46709207118489,8.99746614106264));
#29274=CARTESIAN_POINT('Ctrl Pts',(-2.2981699927958,1.9789494512765,9.57090841885345));
#29275=CARTESIAN_POINT('Ctrl Pts',(-2.27842047188086,0.345494297148205,
9.76724948915638));
#29276=CARTESIAN_POINT('Ctrl Pts',(-2.25867095096591,-1.23615136259958,
9.56279531300263));
#29277=CARTESIAN_POINT('Ctrl Pts',(-2.23892143005097,-2.81779702234732,
9.35834113684888));
#29278=CARTESIAN_POINT('Ctrl Pts',(-2.21917190913603,-4.34763318771457,
8.75309171423847));
#29279=CARTESIAN_POINT('Ctrl Pts',(-2.19942238822108,-5.64104235782824,
7.82008730813342));
#29280=CARTESIAN_POINT('Ctrl Pts',(-2.17967286730614,-6.93445152794191,
6.88708290202836));
#29281=CARTESIAN_POINT('Ctrl Pts',(-2.15992334639119,-7.99143370280202,
5.62632351242866));
#29282=CARTESIAN_POINT('Ctrl Pts',(-2.14017382547625,-8.68443443441755,
4.18995500500241));
#29283=CARTESIAN_POINT('Ctrl Pts',(-2.12228786293019,-9.31204384243555,
2.88912176267674));
#29284=CARTESIAN_POINT('Ctrl Pts',(-2.10440190038413,-9.64112134924384,
1.44425666161893));
#29285=CARTESIAN_POINT('Ctrl Pts',(-2.08651593783807,-9.64217411726438,
-0.000144835560233357));
#29286=CARTESIAN_POINT('Origin',(-3.5,0.,0.));
#29287=CARTESIAN_POINT('',(-1.33651593783807,-9.64079438360302,-9.14169411088817E-5));
#29288=CARTESIAN_POINT('',(-1.53848406216193,-9.64228534650892,9.30951726905646E-5));
#29289=CARTESIAN_POINT('',(-3.5,-9.64155,-1.18074933463192E-15));
#29290=CARTESIAN_POINT('Ctrl Pts',(-1.53848406216193,-9.64228534650892,
9.30951726905646E-5));
#29291=CARTESIAN_POINT('Ctrl Pts',(-1.53962492837896,-9.64233187046965,
0.0922219745249846));
#29292=CARTESIAN_POINT('Ctrl Pts',(-1.54076579459598,-9.64103870036278,
0.184349545103802));
#29293=CARTESIAN_POINT('Ctrl Pts',(-1.541906660813,-9.638397502465,0.276438452957102));
#29294=CARTESIAN_POINT('Ctrl Pts',(-1.56165618172795,-9.59267575845648,
1.87058839319153));
#29295=CARTESIAN_POINT('Ctrl Pts',(-1.58140570264289,-9.1429901340128,3.45315226321777));
#29296=CARTESIAN_POINT('Ctrl Pts',(-1.60115522355784,-8.34360777096442,
4.83314949055984));
#29297=CARTESIAN_POINT('Ctrl Pts',(-1.62090474447278,-7.54422540791601,
6.21314671790196));
#29298=CARTESIAN_POINT('Ctrl Pts',(-1.64065426538773,-6.39514630626289,
7.39057730255991));
#29299=CARTESIAN_POINT('Ctrl Pts',(-1.66040378630267,-5.03503898284049,
8.22335132869036));
#29300=CARTESIAN_POINT('Ctrl Pts',(-1.68015330721762,-3.67493165941809,
9.05612535482081));
#29301=CARTESIAN_POINT('Ctrl Pts',(-1.69990282813256,-2.10379611422641,
9.54424282242376));
#29302=CARTESIAN_POINT('Ctrl Pts',(-1.71965234904751,-0.511233772864205,
9.62879871340552));
#29303=CARTESIAN_POINT('Ctrl Pts',(-1.73940186996245,1.08132856849799,9.71335460438728));
#29304=CARTESIAN_POINT('Ctrl Pts',(-1.7591513908774,2.69531770603071,9.39434891874785));
#29305=CARTESIAN_POINT('Ctrl Pts',(-1.77890091179234,4.13596073022041,8.71027861046198));
#29306=CARTESIAN_POINT('Ctrl Pts',(-1.79865043270729,5.57660375441009,8.02620830217611));
#29307=CARTESIAN_POINT('Ctrl Pts',(-1.81839995362223,6.84390066525676,6.97707337124382));
#29308=CARTESIAN_POINT('Ctrl Pts',(-1.83814947453718,7.78491666239339,5.68948127630161));
#29309=CARTESIAN_POINT('Ctrl Pts',(-1.85789899545212,8.72593265953001,4.4018891813594));
#29310=CARTESIAN_POINT('Ctrl Pts',(-1.87764851636707,9.3406677429566,2.87583992240729));
#29311=CARTESIAN_POINT('Ctrl Pts',(-1.89739803728201,9.55493693955612,1.29549400419403));
#29312=CARTESIAN_POINT('Ctrl Pts',(-1.91714755819696,9.76920613615564,-0.284851914019197));
#29313=CARTESIAN_POINT('Ctrl Pts',(-1.9368970791119,9.5830094459281,-1.91949449149356));
#29314=CARTESIAN_POINT('Ctrl Pts',(-1.95664660002685,9.01881670479375,-3.41116840380682));
#29315=CARTESIAN_POINT('Ctrl Pts',(-1.97639612094179,8.45462396365938,-4.90284231612012));
#29316=CARTESIAN_POINT('Ctrl Pts',(-1.99614564185674,7.51243517161817,-6.25154756327229));
#29317=CARTESIAN_POINT('Ctrl Pts',(-2.01589516277168,6.3059517459036,-7.29452515330038));
#29318=CARTESIAN_POINT('Ctrl Pts',(-2.03564468368663,5.09946832018903,-8.33750274332848));
#29319=CARTESIAN_POINT('Ctrl Pts',(-2.05539420460157,3.62869026080111,-9.07475267623249));
#29320=CARTESIAN_POINT('Ctrl Pts',(-2.07514372551652,2.07110805712042,-9.41730513732711));
#29321=CARTESIAN_POINT('Ctrl Pts',(-2.09489324643146,0.51352585343973,-9.75985759842174));
#29322=CARTESIAN_POINT('Ctrl Pts',(-2.11464276734641,-1.13086049453372,
-9.70771258770698));
#29323=CARTESIAN_POINT('Ctrl Pts',(-2.13439228826135,-2.66360980407379,
-9.26716285847178));
#29324=CARTESIAN_POINT('Ctrl Pts',(-2.1541418091763,-4.19635911361386,-8.82661312923658));
#29325=CARTESIAN_POINT('Ctrl Pts',(-2.17389133009124,-5.61747138472055,
-7.99765868148093));
#29326=CARTESIAN_POINT('Ctrl Pts',(-2.19364085100619,-6.7554496938074,-6.88033604326375));
#29327=CARTESIAN_POINT('Ctrl Pts',(-2.21339037192113,-7.89342800289421,
-5.7630134050466));
#29328=CARTESIAN_POINT('Ctrl Pts',(-2.23313989283608,-8.74827234996121,
-4.35732257636792));
#29329=CARTESIAN_POINT('Ctrl Pts',(-2.25288941375102,-9.21682186682932,
-2.83289945266923));
#29330=CARTESIAN_POINT('Ctrl Pts',(-2.26475429655466,-9.49831148519949,
-1.9170746190575));
#29331=CARTESIAN_POINT('Ctrl Pts',(-2.2766191793583,-9.64037866590084,-0.958396646579831));
#29332=CARTESIAN_POINT('Ctrl Pts',(-2.28848406216193,-9.64087107694564,
0.000138544266770069));
#29333=CARTESIAN_POINT('Ctrl Pts',(-2.08651593783807,-9.64217411726438,
-0.000144835560233357));
#29334=CARTESIAN_POINT('Ctrl Pts',(-2.08465237946918,-9.64228380633759,
-0.150638637119236));
#29335=CARTESIAN_POINT('Ctrl Pts',(-2.0827888211003,-9.63883252828628,-0.301127405892672));
#29336=CARTESIAN_POINT('Ctrl Pts',(-2.08092526273141,-9.63178692444962,
-0.45144770643226));
#29337=CARTESIAN_POINT('Ctrl Pts',(-2.06117574181647,-9.5571193944952,-2.04450428518778));
#29338=CARTESIAN_POINT('Ctrl Pts',(-2.04142622090152,-9.07876504621538,
-3.61863981744596));
#29339=CARTESIAN_POINT('Ctrl Pts',(-2.02167669998658,-8.25445070442347,
-4.98389084530197));
#29340=CARTESIAN_POINT('Ctrl Pts',(-2.00192717907163,-7.43013636263153,
-6.34914187315801));
#29341=CARTESIAN_POINT('Ctrl Pts',(-1.98217765815669,-6.25986202732746,
-7.50550839661188));
#29342=CARTESIAN_POINT('Ctrl Pts',(-1.96242813724174,-4.88485401281266,
-8.31344246766343));
#29343=CARTESIAN_POINT('Ctrl Pts',(-1.9426786163268,-3.50984599829794,-9.12137653871494));
#29344=CARTESIAN_POINT('Ctrl Pts',(-1.92292909541185,-1.9301043045725,-9.58087815736418));
#29345=CARTESIAN_POINT('Ctrl Pts',(-1.90317957449691,-0.336268929645929,
-9.63649560766758));
#29346=CARTESIAN_POINT('Ctrl Pts',(-1.88343005358196,1.25756644528064,-9.69211305797098));
#29347=CARTESIAN_POINT('Ctrl Pts',(-1.86368053266702,2.86549550140836,-9.34384633992854));
#29348=CARTESIAN_POINT('Ctrl Pts',(-1.84393101175207,4.29347664745853,-8.63372356908478));
#29349=CARTESIAN_POINT('Ctrl Pts',(-1.82418149083713,5.72145779350875,-7.92360079824101));
#29350=CARTESIAN_POINT('Ctrl Pts',(-1.80443196992218,6.96949102948142,-6.8516219745959));
#29351=CARTESIAN_POINT('Ctrl Pts',(-1.78468244900724,7.88696625591108,-5.54715131105702));
#29352=CARTESIAN_POINT('Ctrl Pts',(-1.76493292809229,8.80444148234076,-4.24268064751813));
#29353=CARTESIAN_POINT('Ctrl Pts',(-1.74518340717735,9.39135869922739,-2.70571814408551));
#29354=CARTESIAN_POINT('Ctrl Pts',(-1.7254338862624,9.57688993671781,-1.12174129354095));
#29355=CARTESIAN_POINT('Ctrl Pts',(-1.70568436534746,9.76242117420822,0.46223555700355));
#29356=CARTESIAN_POINT('Ctrl Pts',(-1.68593484443251,9.54656643230241,2.09322675465993));
#29357=CARTESIAN_POINT('Ctrl Pts',(-1.66618532351757,8.9553746199649,3.57440761605757));
#29358=CARTESIAN_POINT('Ctrl Pts',(-1.64643580260262,8.36418280762738,5.05558847745521));
#29359=CARTESIAN_POINT('Ctrl Pts',(-1.62668628168768,7.39765392485815,6.38695900259412));
#29360=CARTESIAN_POINT('Ctrl Pts',(-1.60693676077273,6.17242670127939,7.40785211832518));
#29361=CARTESIAN_POINT('Ctrl Pts',(-1.58718723985779,4.94719947770057,8.4287452340563));
#29362=CARTESIAN_POINT('Ctrl Pts',(-1.56743771894284,3.46327391331218,9.13916094037954));
#29363=CARTESIAN_POINT('Ctrl Pts',(-1.5476881980279,1.89972711151983,9.45336772221405));
#29364=CARTESIAN_POINT('Ctrl Pts',(-1.52793867711295,0.336180309727578,
9.76757450404853));
#29365=CARTESIAN_POINT('Ctrl Pts',(-1.50818915619801,-1.30698772946864,
9.68557236139433));
#29366=CARTESIAN_POINT('Ctrl Pts',(-1.48843963528306,-2.83148284635523,
9.21725714518358));
#29367=CARTESIAN_POINT('Ctrl Pts',(-1.46869011436812,-4.35597796324186,
8.74894192897282));
#29368=CARTESIAN_POINT('Ctrl Pts',(-1.44894059345317,-5.76180015781887,
7.89431363920549));
#29369=CARTESIAN_POINT('Ctrl Pts',(-1.42919107253823,-6.87929768167669,
6.75650707070742));
#29370=CARTESIAN_POINT('Ctrl Pts',(-1.40944155162328,-7.99679520553452,
5.61870050220935));
#29371=CARTESIAN_POINT('Ctrl Pts',(-1.38969203070834,-8.82596805867316,
4.19771565498054));
#29372=CARTESIAN_POINT('Ctrl Pts',(-1.36994250979339,-9.26675335631859,
2.66503407535437));
#29373=CARTESIAN_POINT('Ctrl Pts',(-1.35880031914162,-9.51543350628356,
1.80033308122873));
#29374=CARTESIAN_POINT('Ctrl Pts',(-1.34765812848984,-9.64049234473773,
0.90007972103179));
#29375=CARTESIAN_POINT('Ctrl Pts',(-1.33651593783807,-9.64079438360302,
-9.14169411088817E-5));
#29376=CARTESIAN_POINT('Origin',(-3.5,0.,0.));
#29377=CARTESIAN_POINT('',(-0.586515937838063,-9.64158892627347,0.000242834945830858));
#29378=CARTESIAN_POINT('',(-0.788484062161934,-9.64129453877519,-0.000235704550493598));
#29379=CARTESIAN_POINT('',(-3.5,-9.64155,-1.18074933463192E-15));
#29380=CARTESIAN_POINT('Ctrl Pts',(-0.788484062161934,-9.64129453877519,
-0.000235704550493598));
#29381=CARTESIAN_POINT('Ctrl Pts',(-0.802630677399617,-9.64022960846392,
1.14249116596726));
#29382=CARTESIAN_POINT('Ctrl Pts',(-0.816777292637301,-9.43695967827412,
2.2855868580281));
#29383=CARTESIAN_POINT('Ctrl Pts',(-0.830923907874984,-9.03930390030387,
3.35650258926584));
#29384=CARTESIAN_POINT('Ctrl Pts',(-0.850673428789929,-8.48415265231826,
4.85156499655352));
#29385=CARTESIAN_POINT('Ctrl Pts',(-0.870422949704873,-7.55014669543877,
6.20594988869364));
#29386=CARTESIAN_POINT('Ctrl Pts',(-0.890172470619819,-6.3499999590804,
7.25621286577753));
#29387=CARTESIAN_POINT('Ctrl Pts',(-0.909921991534764,-5.14985322272204,
8.30647584286142));
#29388=CARTESIAN_POINT('Ctrl Pts',(-0.929671512449711,-3.6835657068848,
9.0526169048891));
#29389=CARTESIAN_POINT('Ctrl Pts',(-0.949421033364656,-2.12808599133395,
9.40459327388937));
#29390=CARTESIAN_POINT('Ctrl Pts',(-0.969170554279602,-0.572606275783102,
9.75656964288964));
#29391=CARTESIAN_POINT('Ctrl Pts',(-0.988920075194546,1.07206563948137,
9.71438131886251));
#29392=CARTESIAN_POINT('Ctrl Pts',(-1.00866959610949,2.60745411005643,9.28311950250272));
#29393=CARTESIAN_POINT('Ctrl Pts',(-1.02841911702443,4.14284258063145,8.85185768614296));
#29394=CARTESIAN_POINT('Ctrl Pts',(-1.04816863793938,5.56894760651708,8.03152237745056));
#29395=CARTESIAN_POINT('Ctrl Pts',(-1.06791815885432,6.71366974868721,6.92110996440303));
#29396=CARTESIAN_POINT('Ctrl Pts',(-1.08766767976927,7.85839189085738,5.81069755135547));
#29397=CARTESIAN_POINT('Ctrl Pts',(-1.10741720068421,8.72173114931205,4.41020803395276));
#29398=CARTESIAN_POINT('Ctrl Pts',(-1.12716672159916,9.19950150733269,2.8886496240251));
#29399=CARTESIAN_POINT('Ctrl Pts',(-1.1469162425141,9.67727186535334,1.36709121409741));
#29400=CARTESIAN_POINT('Ctrl Pts',(-1.16666576342905,9.76947332293996,-0.275536088355169));
#29401=CARTESIAN_POINT('Ctrl Pts',(-1.186415284344,9.46497919668564,-1.84100337862394));
#29402=CARTESIAN_POINT('Ctrl Pts',(-1.20616480525894,9.16048507043134,-3.40647066889264));
#29403=CARTESIAN_POINT('Ctrl Pts',(-1.22591432617388,8.45929536033612,-4.89477794697749));
#29404=CARTESIAN_POINT('Ctrl Pts',(-1.24566384708883,7.44602820711744,-6.12631933322187));
#29405=CARTESIAN_POINT('Ctrl Pts',(-1.26541336800377,6.43276105389874,-7.3578607194663));
#29406=CARTESIAN_POINT('Ctrl Pts',(-1.28516288891872,5.10741645755655,-8.33263621387025));
#29407=CARTESIAN_POINT('Ctrl Pts',(-1.30491240983366,3.62993429447211,-8.93301190257866));
#29408=CARTESIAN_POINT('Ctrl Pts',(-1.32466193074861,2.15245213138768,-9.53338759128707));
#29409=CARTESIAN_POINT('Ctrl Pts',(-1.34441145166355,0.522832401560974,
-9.75936347429993));
#29410=CARTESIAN_POINT('Ctrl Pts',(-1.3641609725785,-1.06226571757125,-9.58366924403538));
#29411=CARTESIAN_POINT('Ctrl Pts',(-1.38391049349344,-2.64736383670343,
-9.40797501377084));
#29412=CARTESIAN_POINT('Ctrl Pts',(-1.40366001440839,-4.18794034514114,
-8.83061067022889));
#29413=CARTESIAN_POINT('Ctrl Pts',(-1.42340953532333,-5.49808161936687,
-7.92125136203724));
#29414=CARTESIAN_POINT('Ctrl Pts',(-1.44315905623828,-6.80822289359264,
-7.01189205384556));
#29415=CARTESIAN_POINT('Ctrl Pts',(-1.46290857715322,-7.88792893360642,
-5.77053778100414));
#29416=CARTESIAN_POINT('Ctrl Pts',(-1.48265809806817,-8.60690302182664,
-4.3469926393621));
#29417=CARTESIAN_POINT('Ctrl Pts',(-1.50126675276609,-9.28434429253203,
-3.00568111581648));
#29418=CARTESIAN_POINT('Ctrl Pts',(-1.51987540746401,-9.64152649476305,
-1.50261991183219));
#29419=CARTESIAN_POINT('Ctrl Pts',(-1.53848406216193,-9.64228534650892,
9.30951726905646E-5));
#29420=CARTESIAN_POINT('Ctrl Pts',(-1.33651593783807,-9.64079438360302,
-9.14169411088817E-5));
#29421=CARTESIAN_POINT('Ctrl Pts',(-1.3279086075749,-9.64102770830074,-0.695472650313908));
#29422=CARTESIAN_POINT('Ctrl Pts',(-1.31930127731173,-9.56681184096733,
-1.39080481719761));
#29423=CARTESIAN_POINT('Ctrl Pts',(-1.31069394704856,-9.41762333037316,
-2.06966064775193));
#29424=CARTESIAN_POINT('Ctrl Pts',(-1.29094442613361,-9.07531026463006,
-3.62729547920872));
#29425=CARTESIAN_POINT('Ctrl Pts',(-1.27119490521867,-8.33828639099159,
-5.09818683009872));
#29426=CARTESIAN_POINT('Ctrl Pts',(-1.25144538430372,-7.29549424377304,
-6.3048305392545));
#29427=CARTESIAN_POINT('Ctrl Pts',(-1.23169586338878,-6.25270209655455,
-7.51147424841021));
#29428=CARTESIAN_POINT('Ctrl Pts',(-1.21194634247383,-4.90414167575602,
-8.45387031583172));
#29429=CARTESIAN_POINT('Ctrl Pts',(-1.19219682155889,-3.41255449599212,
-9.01829231071637));
#29430=CARTESIAN_POINT('Ctrl Pts',(-1.17244730064394,-1.9209673162282,-9.58271430560103));
#29431=CARTESIAN_POINT('Ctrl Pts',(-1.152697779729,-0.286353377498845,-9.76916222794881));
#29432=CARTESIAN_POINT('Ctrl Pts',(-1.13294825881405,1.29402545183876,-9.55513592366089));
#29433=CARTESIAN_POINT('Ctrl Pts',(-1.11319873789911,2.87440428117639,-9.34110961937297));
#29434=CARTESIAN_POINT('Ctrl Pts',(-1.09344921698416,4.40054800112231,-8.72660908844935));
#29435=CARTESIAN_POINT('Ctrl Pts',(-1.07369969606922,5.68828470756819,-7.78579099869037));
#29436=CARTESIAN_POINT('Ctrl Pts',(-1.05395017515427,6.97602141401403,-6.84497290893142));
#29437=CARTESIAN_POINT('Ctrl Pts',(-1.03420065423933,8.02535110695982,-5.57783726033715));
#29438=CARTESIAN_POINT('Ctrl Pts',(-1.01445113332438,8.70964282428737,-4.13729939247586));
#29439=CARTESIAN_POINT('Ctrl Pts',(-0.994701612409438,9.39393454161492,
-2.69676152461457));
#29440=CARTESIAN_POINT('Ctrl Pts',(-0.974952091494494,9.71318828332421,
-1.08282143748628));
#29441=CARTESIAN_POINT('Ctrl Pts',(-0.95520257057955,9.62887716054125,0.509753878698472));
#29442=CARTESIAN_POINT('Ctrl Pts',(-0.935453049664605,9.54456603775828,
2.10232919488327));
#29443=CARTESIAN_POINT('Ctrl Pts',(-0.91570352874966,9.05669005048304,3.67353974012451));
#29444=CARTESIAN_POINT('Ctrl Pts',(-0.895954007834715,8.22412507545669,
5.03377503796996));
#29445=CARTESIAN_POINT('Ctrl Pts',(-0.876204486919769,7.39156010043033,
6.39401033581541));
#29446=CARTESIAN_POINT('Ctrl Pts',(-0.856454966004824,6.21430613765286,
7.54327038626506));
#29447=CARTESIAN_POINT('Ctrl Pts',(-0.836705445089879,4.83443178860065,
8.34286483595423));
#29448=CARTESIAN_POINT('Ctrl Pts',(-0.816955924174934,3.45455743954846,
9.14245928564339));
#29449=CARTESIAN_POINT('Ctrl Pts',(-0.797206403259989,1.87206270422148,
9.5923881345721));
#29450=CARTESIAN_POINT('Ctrl Pts',(-0.777456882345044,0.27791981206064,
9.63835488907317));
#29451=CARTESIAN_POINT('Ctrl Pts',(-0.757707361430099,-1.31622308010023,
9.68432164357423));
#29452=CARTESIAN_POINT('Ctrl Pts',(-0.737957840515153,-2.922014129095,9.32632630364767));
#29453=CARTESIAN_POINT('Ctrl Pts',(-0.718208319600208,-4.34566975397303,
8.60757101504396));
#29454=CARTESIAN_POINT('Ctrl Pts',(-0.698458798685263,-5.76932537885106,
7.88881572644025));
#29455=CARTESIAN_POINT('Ctrl Pts',(-0.678709277770318,-7.01084557961234,
6.80930048915941));
#29456=CARTESIAN_POINT('Ctrl Pts',(-0.658959756855373,-7.92040623656926,
5.49929899508776));
#29457=CARTESIAN_POINT('Ctrl Pts',(-0.639210235940428,-8.82996689352616,
4.18929750101614));
#29458=CARTESIAN_POINT('Ctrl Pts',(-0.619460715025483,-9.40756800667872,
2.64880975015375));
#29459=CARTESIAN_POINT('Ctrl Pts',(-0.599711194110539,-9.58350585451965,
1.06373865495752));
#29460=CARTESIAN_POINT('Ctrl Pts',(-0.595312775353047,-9.62268899893257,
0.71072723422002));
#29461=CARTESIAN_POINT('Ctrl Pts',(-0.590914356595555,-9.64194972140693,
0.355504488041643));
#29462=CARTESIAN_POINT('Ctrl Pts',(-0.586515937838063,-9.64158892627347,
0.000242834945830858));
#29463=CARTESIAN_POINT('Origin',(-3.5,0.,0.));
#29464=CARTESIAN_POINT('',(0.16348406216194,-9.64208031777467,-0.000174349252608778));
#29465=CARTESIAN_POINT('',(-0.0384840621619312,-9.6409393879154,0.000166496178767295));
#29466=CARTESIAN_POINT('',(-3.5,-9.64155,-1.18074933463192E-15));
#29467=CARTESIAN_POINT('Ctrl Pts',(-0.0384840621619312,-9.6409393879154,
0.000166496178767295));
#29468=CARTESIAN_POINT('Ctrl Pts',(-0.045886905505331,-9.64131207733847,
0.598212169977169));
#29469=CARTESIAN_POINT('Ctrl Pts',(-0.0532897488487309,-9.58653262653383,
1.1961904000962));
#29470=CARTESIAN_POINT('Ctrl Pts',(-0.0606925921921309,-9.47595184764967,
1.7836651068862));
#29471=CARTESIAN_POINT('Ctrl Pts',(-0.0804421131070762,-9.18094122753292,
3.35094722681577));
#29472=CARTESIAN_POINT('Ctrl Pts',(-0.100191634022022,-8.48877513866814,
4.84347249283488));
#29473=CARTESIAN_POINT('Ctrl Pts',(-0.119941154936967,-7.48298276944078,
6.08112600652889));
#29474=CARTESIAN_POINT('Ctrl Pts',(-0.139690675851912,-6.47719040021342,
7.3187795202229));
#29475=CARTESIAN_POINT('Ctrl Pts',(-0.159440196766856,-5.1577717506235,
8.30156128159181));
#29476=CARTESIAN_POINT('Ctrl Pts',(-0.179189717681801,-3.68395156600086,
8.91087119716035));
#29477=CARTESIAN_POINT('Ctrl Pts',(-0.198939238596746,-2.21013138137827,
9.52018111272887));
#29478=CARTESIAN_POINT('Ctrl Pts',(-0.218688759511691,-0.581909661722974,
9.75601918249705));
#29479=CARTESIAN_POINT('Ctrl Pts',(-0.238438280426636,1.00422312458321,
9.58992495018725));
#29480=CARTESIAN_POINT('Ctrl Pts',(-0.258187801341581,2.59035591088944,
9.42383071787745));
#29481=CARTESIAN_POINT('Ctrl Pts',(-0.277937322256526,4.13439976384655,
8.85580418348966));
#29482=CARTESIAN_POINT('Ctrl Pts',(-0.297686843171471,5.45002262786544,
7.95439362801577));
#29483=CARTESIAN_POINT('Ctrl Pts',(-0.317436364086416,6.76564549188433,
7.05298307254187));
#29484=CARTESIAN_POINT('Ctrl Pts',(-0.337185885001362,7.85284736696499,
5.81818849598189));
#29485=CARTESIAN_POINT('Ctrl Pts',(-0.356935405916307,8.58042695348651,
4.39902238340523));
#29486=CARTESIAN_POINT('Ctrl Pts',(-0.376684926831252,9.308006540008,2.97985627082861));
#29487=CARTESIAN_POINT('Ctrl Pts',(-0.396434447746196,9.67596383797037,
1.37631862223533));
#29488=CARTESIAN_POINT('Ctrl Pts',(-0.41618396866114,9.63989451289301,-0.218078917157266));
#29489=CARTESIAN_POINT('Ctrl Pts',(-0.435933489576085,9.60382518781565,
-1.81247645654993));
#29490=CARTESIAN_POINT('Ctrl Pts',(-0.455683010491032,9.16372923969851,
-3.39773388674197));
#29491=CARTESIAN_POINT('Ctrl Pts',(-0.475432531405977,8.37271654784118,
-4.78254558193465));
#29492=CARTESIAN_POINT('Ctrl Pts',(-0.495182052320922,7.58170385598388,
-6.16735727712726));
#29493=CARTESIAN_POINT('Ctrl Pts',(-0.514931573235866,6.43977442038642,
-7.35172323732058));
#29494=CARTESIAN_POINT('Ctrl Pts',(-0.534681094150811,5.08473395079955,
-8.19271659972427));
#29495=CARTESIAN_POINT('Ctrl Pts',(-0.554430615065756,3.72969348121264,
-9.03370996212798));
#29496=CARTESIAN_POINT('Ctrl Pts',(-0.574180135980702,2.16154197763633,
-9.53133072674204));
#29497=CARTESIAN_POINT('Ctrl Pts',(-0.593929656895646,0.569520757628604,
-9.62552703702085));
#29498=CARTESIAN_POINT('Ctrl Pts',(-0.613679177810591,-1.02250046237912,
-9.71972334729966));
#29499=CARTESIAN_POINT('Ctrl Pts',(-0.633428698725536,-2.63839139881825,
-9.41049520324323));
#29500=CARTESIAN_POINT('Ctrl Pts',(-0.653178219640481,-4.08314963697168,
-8.73515962509546));
#29501=CARTESIAN_POINT('Ctrl Pts',(-0.672927740555426,-5.52790787512507,
-8.05982404694771));
#29502=CARTESIAN_POINT('Ctrl Pts',(-0.692677261470371,-6.80153341499276,
-7.01838103470866));
#29503=CARTESIAN_POINT('Ctrl Pts',(-0.712426782385315,-7.75032773019536,
-5.73650980199293));
#29504=CARTESIAN_POINT('Ctrl Pts',(-0.73217630330026,-8.69912204539795,
-4.45463856927719));
#29505=CARTESIAN_POINT('Ctrl Pts',(-0.751925824215204,-9.32308513593545,
-2.93233911608478));
#29506=CARTESIAN_POINT('Ctrl Pts',(-0.771675345130148,-9.54691841165834,
-1.35331942827096));
#29507=CARTESIAN_POINT('Ctrl Pts',(-0.77727825080741,-9.61041953336701,
-0.905354213749452));
#29508=CARTESIAN_POINT('Ctrl Pts',(-0.782881156484672,-9.64171631486697,
-0.452823886444953));
#29509=CARTESIAN_POINT('Ctrl Pts',(-0.788484062161934,-9.64129453877519,
-0.000235704550493598));
#29510=CARTESIAN_POINT('Ctrl Pts',(-0.586515937838063,-9.64158892627347,
0.000242834945830858));
#29511=CARTESIAN_POINT('Ctrl Pts',(-0.57116483568061,-9.64032970034318,
-1.2396704679906));
#29512=CARTESIAN_POINT('Ctrl Pts',(-0.555813733523157,-9.40005910021102,
-2.48005769939615));
#29513=CARTESIAN_POINT('Ctrl Pts',(-0.540462631365704,-8.93356968403343,
-3.62856129754286));
#29514=CARTESIAN_POINT('Ctrl Pts',(-0.52071311045076,-8.333421083177,-5.10613571531682));
#29515=CARTESIAN_POINT('Ctrl Pts',(-0.500963589535815,-7.35884929893488,
-6.43163011133468));
#29516=CARTESIAN_POINT('Ctrl Pts',(-0.481214068620871,-6.1274636618099,
-7.4450865316139));
#29517=CARTESIAN_POINT('Ctrl Pts',(-0.461464547705925,-4.89607802468489,
-8.45854295189315));
#29518=CARTESIAN_POINT('Ctrl Pts',(-0.44171502679098,-3.40787853467704,
-9.15996139643373));
#29519=CARTESIAN_POINT('Ctrl Pts',(-0.421965505876035,-1.84245806384899,
-9.46469612147266));
#29520=CARTESIAN_POINT('Ctrl Pts',(-0.402215984961089,-0.277037593020945,
-9.76943084651159));
#29521=CARTESIAN_POINT('Ctrl Pts',(-0.382466464046144,1.36560385862727,
-9.67748185204887));
#29522=CARTESIAN_POINT('Ctrl Pts',(-0.362716943131199,2.88723567898901,
-9.19994535444941));
#29523=CARTESIAN_POINT('Ctrl Pts',(-0.342967422216254,4.40886749935072,
-8.72240885684995));
#29524=CARTESIAN_POINT('Ctrl Pts',(-0.32321790130131,5.80948968842594,-7.85928485611378));
#29525=CARTESIAN_POINT('Ctrl Pts',(-0.303468380386366,6.92007802364878,
-6.71473339269328));
#29526=CARTESIAN_POINT('Ctrl Pts',(-0.283718859471421,8.03066635887166,
-5.57018192927274));
#29527=CARTESIAN_POINT('Ctrl Pts',(-0.263969338556473,8.85122084024217,
-4.14420300316775));
#29528=CARTESIAN_POINT('Ctrl Pts',(-0.244219817641528,9.28271863083791,
-2.60888083479162));
#29529=CARTESIAN_POINT('Ctrl Pts',(-0.224470296726584,9.71421642143363,
-1.07355866641553));
#29530=CARTESIAN_POINT('Ctrl Pts',(-0.204720775811639,9.75665752125467,
0.571106744231792));
#29531=CARTESIAN_POINT('Ctrl Pts',(-0.184971254896695,9.40492022443375,
2.12664053549246));
#29532=CARTESIAN_POINT('Ctrl Pts',(-0.16522173398175,9.05318292761283,3.68217432675312));
#29533=CARTESIAN_POINT('Ctrl Pts',(-0.145472213066806,8.30726723414997,
5.1485764986271));
#29534=CARTESIAN_POINT('Ctrl Pts',(-0.125722692151861,7.25718872636263,
6.34888463917673));
#29535=CARTESIAN_POINT('Ctrl Pts',(-0.105973171236915,6.20711021857523,
7.54919277972643));
#29536=CARTESIAN_POINT('Ctrl Pts',(-0.0862236503219702,4.85286889646334,
8.48340688895172));
#29537=CARTESIAN_POINT('Ctrl Pts',(-0.0664741294070245,3.35789183156476,
9.03878790976793));
#29538=CARTESIAN_POINT('Ctrl Pts',(-0.0467246084920799,1.86291476666626,
9.5941689305841));
#29539=CARTESIAN_POINT('Ctrl Pts',(-0.0269750875771353,0.22720195898112,
9.77071686299123));
#29540=CARTESIAN_POINT('Ctrl Pts',(-0.00722556666219065,-1.35185210879035,
9.54712627940369));
#29541=CARTESIAN_POINT('Ctrl Pts',(0.0125239542527545,-2.93090617656187,
9.32353569581614));
#29542=CARTESIAN_POINT('Ctrl Pts',(0.0322734751676994,-4.45330150441969,
8.69980659623389));
#29543=CARTESIAN_POINT('Ctrl Pts',(0.0520229960826446,-5.73531854636519,
7.75120930243113));
#29544=CARTESIAN_POINT('Ctrl Pts',(0.0717725169975898,-7.01733558831068,
6.80261200862837));
#29545=CARTESIAN_POINT('Ctrl Pts',(0.0915220379125351,-8.05897434434382,
5.52914652060512));
#29546=CARTESIAN_POINT('Ctrl Pts',(0.11127155882748,-8.73453195993958,4.08449210952313));
#29547=CARTESIAN_POINT('Ctrl Pts',(0.128675726605634,-9.32986377260853,
2.81139754382694));
#29548=CARTESIAN_POINT('Ctrl Pts',(0.146079894383787,-9.64089958585323,
1.40535888296871));
#29549=CARTESIAN_POINT('Ctrl Pts',(0.16348406216194,-9.64208031777467,-0.000174349252608778));
#29550=CARTESIAN_POINT('Origin',(-3.5,0.,0.));
#29551=CARTESIAN_POINT('',(0.913484062161936,-9.64080718149228,-0.000193112876372633));
#29552=CARTESIAN_POINT('',(0.711515937838069,-9.64233463315361,5.55577575209881E-5));
#29553=CARTESIAN_POINT('',(-3.5,-9.64155,-1.18074933463192E-15));
#29554=CARTESIAN_POINT('',(1.,-7.21801009705401,-6.39216838336776));
#29555=CARTESIAN_POINT('Ctrl Pts',(0.913484062161936,-9.64080718149228,
-0.000193112876372633));
#29556=CARTESIAN_POINT('Ctrl Pts',(0.922573187193013,-9.64097580048578,
-0.734553316280234));
#29557=CARTESIAN_POINT('Ctrl Pts',(0.93166231222409,-9.55814059309284,-1.46884207590725));
#29558=CARTESIAN_POINT('Ctrl Pts',(0.940751437255168,-9.39189433566671,
-2.18363780626507));
#29559=CARTESIAN_POINT('Ctrl Pts',(0.960500958170112,-9.03066221190976,
-3.73679866370149));
#29560=CARTESIAN_POINT('Ctrl Pts',(0.980250479085056,-8.27561480792393,
-5.1979255186751));
#29561=CARTESIAN_POINT('Ctrl Pts',(1.,-7.21801009705401,-6.39216838336776));
#29562=CARTESIAN_POINT('',(0.999999999999999,7.21857426272793,-6.39248696093098));
#29563=CARTESIAN_POINT('Origin',(1.,0.,0.));
#29564=CARTESIAN_POINT('Ctrl Pts',(0.999999999999999,7.21857426272793,-6.39248696093098));
#29565=CARTESIAN_POINT('Ctrl Pts',(0.982177658156687,6.26356489870851,-7.46927130190886));
#29566=CARTESIAN_POINT('Ctrl Pts',(0.964355316313374,5.06448313860702,-8.33050693920671));
#29567=CARTESIAN_POINT('Ctrl Pts',(0.946532974470062,3.73783082533989,-8.88839338664454));
#29568=CARTESIAN_POINT('Ctrl Pts',(0.926783453555117,2.26772393152777,-9.50660563724011));
#29569=CARTESIAN_POINT('Ctrl Pts',(0.907033932640172,0.640965728191514,
-9.75231775629702));
#29570=CARTESIAN_POINT('Ctrl Pts',(0.887284411725227,-0.946142180621593,
-9.59583455469918));
#29571=CARTESIAN_POINT('Ctrl Pts',(0.867534890810282,-2.5332500894347,-9.43935135310134));
#29572=CARTESIAN_POINT('Ctrl Pts',(0.847785369895337,-4.08070770372466,
-8.88067283084875));
#29573=CARTESIAN_POINT('Ctrl Pts',(0.828035848980391,-5.40176465919483,
-7.98724151005226));
#29574=CARTESIAN_POINT('Ctrl Pts',(0.808286328065446,-6.72282161466503,
-7.09381018925575));
#29575=CARTESIAN_POINT('Ctrl Pts',(0.7885368071505,-7.81747791131544,-5.86562606991532));
#29576=CARTESIAN_POINT('Ctrl Pts',(0.768787286235554,-8.55363594974757,
-4.45089233265519));
#29577=CARTESIAN_POINT('Ctrl Pts',(0.749696836769726,-9.26522727857401,
-3.08337040465096));
#29578=CARTESIAN_POINT('Ctrl Pts',(0.730606387303897,-9.64184836527695,
-1.54154199328144));
#29579=CARTESIAN_POINT('Ctrl Pts',(0.711515937838069,-9.64233463315361,
5.55577575209881E-5));
#29580=CARTESIAN_POINT('Origin',(-9.65625985035617,0.,0.));
#29581=CARTESIAN_POINT('',(0.406259850356178,-10.0626034466932,-0.000181953202540996));
#29582=CARTESIAN_POINT('',(0.468740149643834,-10.06286885361,5.79808157464514E-5));
#29583=CARTESIAN_POINT('',(-9.65625985035617,-10.06205,-4.69647557663214E-13));
#29584=CARTESIAN_POINT('',(1.,2.60344811511698,9.71940883564396));
#29585=CARTESIAN_POINT('Ctrl Pts',(0.468740149643834,-10.06286885361,5.79808157466586E-5));
#29586=CARTESIAN_POINT('Ctrl Pts',(0.487830599109663,-10.0623613779771,
-1.60877375665718));
#29587=CARTESIAN_POINT('Ctrl Pts',(0.526670569490437,-9.26269841475242,
-4.88247010492393));
#29588=CARTESIAN_POINT('Ctrl Pts',(0.585260060786157,-5.87362828986304,
-8.68494410471449));
#29589=CARTESIAN_POINT('Ctrl Pts',(0.644508623530991,-1.02878615726,-10.4340771460299));
#29590=CARTESIAN_POINT('Ctrl Pts',(0.703757186275826,4.0643334282463,-9.66479182544668));
#29591=CARTESIAN_POINT('Ctrl Pts',(0.763005749020661,8.1765526549945,-6.56302991227287));
#29592=CARTESIAN_POINT('Ctrl Pts',(0.822254311765496,10.3152148975558,-1.8768974633799));
#29593=CARTESIAN_POINT('Ctrl Pts',(0.88150287451033,9.96442833619652,3.26156383705692));
#29594=CARTESIAN_POINT('Ctrl Pts',(0.940751437255166,7.20829597612923,7.61418408655239));
#29595=CARTESIAN_POINT('Ctrl Pts',(0.980250479085055,4.21155540437341,9.28866001522528));
#29596=CARTESIAN_POINT('Ctrl Pts',(1.,2.60344811511698,9.71940883564396));
#29597=CARTESIAN_POINT('',(0.999999999999999,-2.60375578640692,9.7200109471421));
#29598=CARTESIAN_POINT('Origin',(1.,0.,0.));
#29599=CARTESIAN_POINT('Ctrl Pts',(0.406259850356178,-10.0626034466932,
-0.000181953202541413));
#29600=CARTESIAN_POINT('Ctrl Pts',(0.408605203492968,-10.0627694993772,
-0.197849655297783));
#29601=CARTESIAN_POINT('Ctrl Pts',(0.430700077544703,-10.0090126457275,
-2.05992802286849));
#29602=CARTESIAN_POINT('Ctrl Pts',(0.472544472511383,-8.90922609310004,
-5.52753257240065));
#29603=CARTESIAN_POINT('Ctrl Pts',(0.531793035256219,-5.20171515149495,
-9.10330010082978));
#29604=CARTESIAN_POINT('Ctrl Pts',(0.591041598001052,-0.23874007198555,
-10.4819341046316));
#29605=CARTESIAN_POINT('Ctrl Pts',(0.650290160745889,4.78185742115312,-9.33068794050316));
#29606=CARTESIAN_POINT('Ctrl Pts',(0.709538723490722,8.64832326230869,-5.92743167035388));
#29607=CARTESIAN_POINT('Ctrl Pts',(0.768787286235557,10.4274692096169,-1.09354201610874));
#29608=CARTESIAN_POINT('Ctrl Pts',(0.828035848980392,9.68987600895932,4.00425592589309));
#29609=CARTESIAN_POINT('Ctrl Pts',(0.887284411725228,6.61358904227201,8.1356504120078));
#29610=CARTESIAN_POINT('Ctrl Pts',(0.94460579539843,2.09302808608892,10.2328567692711));
#29611=CARTESIAN_POINT('Ctrl Pts',(0.982177658156686,-1.15257241662438,
10.1075740191406));
#29612=CARTESIAN_POINT('Ctrl Pts',(0.999999999999999,-2.60375578640692,
9.7200109471421));
#29613=CARTESIAN_POINT('Origin',(-9.65625985035617,0.,0.));
#29614=CARTESIAN_POINT('',(-0.343740149643824,-10.0620906239775,0.00025342578346299));
#29615=CARTESIAN_POINT('',(-0.281259850356166,-10.0614127570955,0.000173757629795403));
#29616=CARTESIAN_POINT('',(-9.65625985035617,-10.06205,-4.69647557663214E-13));
#29617=CARTESIAN_POINT('Ctrl Pts',(-0.281259850356166,-10.0614127570955,
0.000173757629795546));
#29618=CARTESIAN_POINT('Ctrl Pts',(-0.268913172784621,-10.0607640655635,
-1.04076580315036));
#29619=CARTESIAN_POINT('Ctrl Pts',(-0.236816974298132,-9.64287151587488,
-3.74728231997338));
#29620=CARTESIAN_POINT('Ctrl Pts',(-0.184971254896697,-7.25443294882962,
-7.56975066843671));
#29621=CARTESIAN_POINT('Ctrl Pts',(-0.125722692151862,-2.7740584993699,
-10.1110099362393));
#29622=CARTESIAN_POINT('Ctrl Pts',(-0.0664741294070278,2.37585137208773,
-10.211917205029));
#29623=CARTESIAN_POINT('Ctrl Pts',(-0.00722556666219231,6.95233546092519,
-7.848117856984));
#29624=CARTESIAN_POINT('Ctrl Pts',(0.0520229960826416,9.85083230810637,
-3.59012893818949));
#29625=CARTESIAN_POINT('Ctrl Pts',(0.111271558827477,10.3717725107696,1.53435894975116));
#29626=CARTESIAN_POINT('Ctrl Pts',(0.170520121572311,8.38942417794793,6.28851998843207));
#29627=CARTESIAN_POINT('Ctrl Pts',(0.229768684317148,4.38223859253949,9.52491003146027));
#29628=CARTESIAN_POINT('Ctrl Pts',(0.289017247061982,-0.682625920371043,
10.4624058141013));
#29629=CARTESIAN_POINT('Ctrl Pts',(0.348265809806817,-5.58273513680522,
8.8747398847227));
#29630=CARTESIAN_POINT('Ctrl Pts',(0.407514372551651,-9.13541725268214,
5.14509959176606));
#29631=CARTESIAN_POINT('Ctrl Pts',(0.447672485830657,-10.0489412906938,
1.7755089194844));
#29632=CARTESIAN_POINT('Ctrl Pts',(0.468081078194718,-10.0628863735066,
0.0556006785662035));
#29633=CARTESIAN_POINT('Ctrl Pts',(0.468740149643834,-10.06286885361,5.79808157466586E-5));
#29634=CARTESIAN_POINT('Ctrl Pts',(-0.343740149643824,-10.0620906239775,
0.000253425783462886));
#29635=CARTESIAN_POINT('Ctrl Pts',(-0.328389047486372,-10.0607764790244,
-1.29373661210569));
#29636=CARTESIAN_POINT('Ctrl Pts',(-0.293288424413976,-9.48743216442293,
-4.25360338997758));
#29637=CARTESIAN_POINT('Ctrl Pts',(-0.238438280426636,-6.66271704930368,
-8.09543845639));
#29638=CARTESIAN_POINT('Ctrl Pts',(-0.1791897176818,-2.00340262005729,-10.2914673500501));
#29639=CARTESIAN_POINT('Ctrl Pts',(-0.119941154936964,3.13944487393184,
-10.0035897640602));
#29640=CARTESIAN_POINT('Ctrl Pts',(-0.0606925921921299,7.52456878997794,
-7.3012866535828));
#29641=CARTESIAN_POINT('Ctrl Pts',(-0.00144402944729414,10.0935935482191,
-2.83677485203218));
#29642=CARTESIAN_POINT('Ctrl Pts',(0.0578045332975393,10.2264698394132,
2.3124093336654));
#29643=CARTESIAN_POINT('Ctrl Pts',(0.117053096042374,7.89112718079254,6.90347984831441));
#29644=CARTESIAN_POINT('Ctrl Pts',(0.176301658787208,3.65121433633638,9.82835471108965));
#29645=CARTESIAN_POINT('Ctrl Pts',(0.235550221532044,-1.46994068227644,
10.3810980324261));
#29646=CARTESIAN_POINT('Ctrl Pts',(0.294798784276879,-6.23631680707128,
8.42830204429616));
#29647=CARTESIAN_POINT('Ctrl Pts',(0.351701993884924,-9.36842634388113,
4.59911138032189));
#29648=CARTESIAN_POINT('Ctrl Pts',(0.388855682578024,-10.0613712191333,
1.46665124885246));
#29649=CARTESIAN_POINT('Ctrl Pts',(0.406259850356178,-10.0626034466932,
-0.000181953202541413));
#29650=CARTESIAN_POINT('Origin',(-9.65625985035617,0.,0.));
#29651=CARTESIAN_POINT('',(-1.09374014964383,-10.0612614286637,-9.54039379347238E-5));
#29652=CARTESIAN_POINT('',(-1.03125985035617,-10.0617833972632,-0.000245984408346792));
#29653=CARTESIAN_POINT('',(-9.65625985035617,-10.06205,-4.69647557663214E-13));
#29654=CARTESIAN_POINT('Ctrl Pts',(-1.03125985035617,-10.0617833972632,
-0.000245984408347166));
#29655=CARTESIAN_POINT('Ctrl Pts',(-1.02565694467891,-10.0622235684104,
-0.472573039252344));
#29656=CARTESIAN_POINT('Ctrl Pts',(-1.0003045180867,-9.91443341033051,-2.60951892962658));
#29657=CARTESIAN_POINT('Ctrl Pts',(-0.955202570579548,-8.42734344184841,
-6.23761212968768));
#29658=CARTESIAN_POINT('Ctrl Pts',(-0.895954007834717,-4.43982570971225,
-9.49820352670374));
#29659=CARTESIAN_POINT('Ctrl Pts',(-0.836705445089881,0.619270202354978,
-10.4663473563483));
#29660=CARTESIAN_POINT('Ctrl Pts',(-0.777456882345046,5.52890159042847,
-8.90837638241207));
#29661=CARTESIAN_POINT('Ctrl Pts',(-0.71820831960021,9.10409989696232,-5.20031610898184));
#29662=CARTESIAN_POINT('Ctrl Pts',(-0.658959756855376,10.4819698768157,
-0.237128802336295));
#29663=CARTESIAN_POINT('Ctrl Pts',(-0.599711194110542,9.32995446540496,
4.78329094252682));
#29664=CARTESIAN_POINT('Ctrl Pts',(-0.540462631365705,5.92609939215782,
8.64923514311966));
#29665=CARTESIAN_POINT('Ctrl Pts',(-0.481214068620872,1.09194519994383,
10.4276353143587));
#29666=CARTESIAN_POINT('Ctrl Pts',(-0.421965505876034,-4.0057564209339,
9.68926406183886));
#29667=CARTESIAN_POINT('Ctrl Pts',(-0.362716943131203,-8.13664505080342,
6.61233165305132));
#29668=CARTESIAN_POINT('Ctrl Pts',(-0.315815057957911,-9.85211717613616,
2.9132404502305));
#29669=CARTESIAN_POINT('Ctrl Pts',(-0.288662693699566,-10.0618017007414,
0.624302188436377));
#29670=CARTESIAN_POINT('Ctrl Pts',(-0.281259850356166,-10.0614127570955,
0.000173757629795546));
#29671=CARTESIAN_POINT('Ctrl Pts',(-1.09374014964383,-10.0612614286637,
-9.54039379352789E-5));
#29672=CARTESIAN_POINT('Ctrl Pts',(-1.08513281938066,-10.061504929426,-0.725804521170841));
#29673=CARTESIAN_POINT('Ctrl Pts',(-1.05677596820255,-9.80633710117914,
-3.11648464536511));
#29674=CARTESIAN_POINT('Ctrl Pts',(-1.00866959610949,-7.93277880763296,
-6.85557748609057));
#29675=CARTESIAN_POINT('Ctrl Pts',(-0.949421033364655,-3.7106519560076,
-9.80606875052385));
#29676=CARTESIAN_POINT('Ctrl Pts',(-0.890172470619817,1.40706267976922,
-10.3898073559533));
#29677=CARTESIAN_POINT('Ctrl Pts',(-0.830923907874984,6.18517442029282,
-8.46590453933774));
#29678=CARTESIAN_POINT('Ctrl Pts',(-0.771675345130147,9.47045775240396,
-4.49870561812545));
#29679=CARTESIAN_POINT('Ctrl Pts',(-0.712426782385315,10.4699901237859,
0.554282496966878));
#29680=CARTESIAN_POINT('Ctrl Pts',(-0.65317821964048,8.94252848812691,5.47349125491902));
#29681=CARTESIAN_POINT('Ctrl Pts',(-0.593929656895644,5.25673474038977,
9.07164054335094));
#29682=CARTESIAN_POINT('Ctrl Pts',(-0.53468109415081,0.302196989220137,
10.4802957619713));
#29683=CARTESIAN_POINT('Ctrl Pts',(-0.475432531405974,-4.72527779166189,
9.35946964684205));
#29684=CARTESIAN_POINT('Ctrl Pts',(-0.41618396866114,-8.61227884524871,
5.97968020636365));
#29685=CARTESIAN_POINT('Ctrl Pts',(-0.372286508073756,-9.95211121964369,
2.40628792237205));
#29686=CARTESIAN_POINT('Ctrl Pts',(-0.348138568401317,-10.0624671545843,
0.371009218838945));
#29687=CARTESIAN_POINT('Ctrl Pts',(-0.343740149643824,-10.0620906239775,
0.000253425783462886));
#29688=CARTESIAN_POINT('Origin',(-9.65625985035617,0.,0.));
#29689=CARTESIAN_POINT('',(-1.84374014964383,-10.06270133709,-0.000151152320359005));
#29690=CARTESIAN_POINT('',(-1.78125985035617,-10.0628174174111,9.71553621948886E-5));
#29691=CARTESIAN_POINT('',(-9.65625985035617,-10.06205,-4.69647557663214E-13));
#29692=CARTESIAN_POINT('Ctrl Pts',(-1.78125985035617,-10.0628174174111,
9.71553621948243E-5));
#29693=CARTESIAN_POINT('Ctrl Pts',(-1.76265119565825,-10.0620254696216,
-1.56815415403654));
#29694=CARTESIAN_POINT('Ctrl Pts',(-1.72429302004538,-9.2936519492452,-4.80155274286011));
#29695=CARTESIAN_POINT('Ctrl Pts',(-1.66618532351757,-5.97835648900369,
-8.61319779510975));
#29696=CARTESIAN_POINT('Ctrl Pts',(-1.60693676077273,-1.15505799756011,
-10.4208331523717));
#29697=CARTESIAN_POINT('Ctrl Pts',(-1.5476881980279,3.94702056942422,-9.71333882822164));
#29698=CARTESIAN_POINT('Ctrl Pts',(-1.48843963528306,8.0964623901765,-6.66147275996483));
#29699=CARTESIAN_POINT('Ctrl Pts',(-1.42919107253823,10.2917751528953,-2.00182086349988));
#29700=CARTESIAN_POINT('Ctrl Pts',(-1.36994250979339,10.0031071452691,3.14098233162225));
#29701=CARTESIAN_POINT('Ctrl Pts',(-1.31069394704856,7.30013009732543,7.52569087389453));
#29702=CARTESIAN_POINT('Ctrl Pts',(-1.25144538430372,2.83522349754239,10.0940294375576));
#29703=CARTESIAN_POINT('Ctrl Pts',(-1.19219682155889,-2.31398105307032,
10.2261143281957));
#29704=CARTESIAN_POINT('Ctrl Pts',(-1.13294825881405,-6.90469259801799,
7.89006607666695));
#29705=CARTESIAN_POINT('Ctrl Pts',(-1.07930260174648,-9.55238338000605,
4.05069827845285));
#29706=CARTESIAN_POINT('Ctrl Pts',(-1.04540646559385,-10.0606720218061,
1.19231899814043));
#29707=CARTESIAN_POINT('Ctrl Pts',(-1.03125985035617,-10.0617833972632,
-0.000245984408347166));
#29708=CARTESIAN_POINT('Ctrl Pts',(-1.84374014964383,-10.06270133709,-0.000151152320359421));
#29709=CARTESIAN_POINT('Ctrl Pts',(-1.84187659127494,-10.0628158100678,
-0.157208488119574));
#29710=CARTESIAN_POINT('Ctrl Pts',(-1.82026351199111,-10.0210430463493,
-1.97865888614579));
#29711=CARTESIAN_POINT('Ctrl Pts',(-1.77890091179234,-8.97550315697813,
-5.41924951978578));
#29712=CARTESIAN_POINT('Ctrl Pts',(-1.71965234904751,-5.31156150582896,
-9.03964803786181));
#29713=CARTESIAN_POINT('Ctrl Pts',(-1.66040378630267,-0.365643087312114,
-10.4782740664349));
#29714=CARTESIAN_POINT('Ctrl Pts',(-1.60115522355784,4.66852545173299,-9.38790670943975));
#29715=CARTESIAN_POINT('Ctrl Pts',(-1.541906660813,8.57591777620947,-6.03171257391441));
#29716=CARTESIAN_POINT('Ctrl Pts',(-1.48265809806816,10.4134616510556,-1.2197289537503));
#29717=CARTESIAN_POINT('Ctrl Pts',(-1.42340953532333,9.73765499990719,3.88664345951686));
#29718=CARTESIAN_POINT('Ctrl Pts',(-1.3641609725785,6.71160775287686,8.05495149893194));
#29719=CARTESIAN_POINT('Ctrl Pts',(-1.30491240983366,2.06567430073889,10.2791493792964));
#29720=CARTESIAN_POINT('Ctrl Pts',(-1.24566384708883,-3.07882185458713,
10.022413794408));
#29721=CARTESIAN_POINT('Ctrl Pts',(-1.18641528434399,-7.48022615564147,
7.34670939530617));
#29722=CARTESIAN_POINT('Ctrl Pts',(-1.13577405186233,-9.69909887236656,
3.54414338453905));
#29723=CARTESIAN_POINT('Ctrl Pts',(-1.1048823402956,-10.060946216881,0.939335185421873));
#29724=CARTESIAN_POINT('Ctrl Pts',(-1.09374014964383,-10.0612614286637,
-9.54039379352789E-5));
#29725=CARTESIAN_POINT('Origin',(-9.65625985035617,0.,0.));
#29726=CARTESIAN_POINT('',(-2.59374014964383,-10.0619647730755,0.000254798100391557));
#29727=CARTESIAN_POINT('',(-2.53125985035617,-10.0613414668576,0.000144586642133095));
#29728=CARTESIAN_POINT('',(-9.65625985035617,-10.06205,-4.69647557663214E-13));
#29729=CARTESIAN_POINT('Ctrl Pts',(-2.53125985035617,-10.0613414668576,
0.000144586642132558));
#29730=CARTESIAN_POINT('Ctrl Pts',(-2.51939496755253,-10.0608275801326,
-1.0001955056727));
#29731=CARTESIAN_POINT('Ctrl Pts',(-2.48778056383395,-9.66577498641524,
-3.6660344256632));
#29732=CARTESIAN_POINT('Ctrl Pts',(-2.43641663920042,-7.34555965317983,
-7.48135522140693));
#29733=CARTESIAN_POINT('Ctrl Pts',(-2.37716807645559,-2.8962845695608,-10.0766789300553));
#29734=CARTESIAN_POINT('Ctrl Pts',(-2.31791951371075,2.25202591556642,-10.2399366132273));
#29735=CARTESIAN_POINT('Ctrl Pts',(-2.25867095096592,6.85679663369709,-7.93172506403346));
#29736=CARTESIAN_POINT('Ctrl Pts',(-2.19942238822108,9.80663895208724,-3.70914478427321));
#29737=CARTESIAN_POINT('Ctrl Pts',(-2.14017382547625,10.3895909899559,1.40865951483102));
#29738=CARTESIAN_POINT('Ctrl Pts',(-2.08092526273141,8.46495382699166,6.18647551310075));
#29739=CARTESIAN_POINT('Ctrl Pts',(-2.02167669998658,4.49725001947583,9.47114907651764));
#29740=CARTESIAN_POINT('Ctrl Pts',(-1.96242813724174,-0.555891664582547,
10.4699048240442));
#29741=CARTESIAN_POINT('Ctrl Pts',(-1.90317957449691,-5.47486560938269,
8.941687152126));
#29742=CARTESIAN_POINT('Ctrl Pts',(-1.84393101175207,-9.072448376092,5.25534042954797));
#29743=CARTESIAN_POINT('Ctrl Pts',(-1.80329110370516,-10.0381540192056,
1.85676423142571));
#29744=CARTESIAN_POINT('Ctrl Pts',(-1.78240071657319,-10.0628659704362,
0.0962440809588831));
#29745=CARTESIAN_POINT('Ctrl Pts',(-1.78125985035617,-10.0628174174111,
9.71553621948243E-5));
#29746=CARTESIAN_POINT('Ctrl Pts',(-2.59374014964383,-10.0619647730755,
0.000254798100391383));
#29747=CARTESIAN_POINT('Ctrl Pts',(-2.57887084225428,-10.0607159489408,
-1.25316844709838));
#29748=CARTESIAN_POINT('Ctrl Pts',(-2.54425201394979,-9.51384009969817,
-4.1724567398586));
#29749=CARTESIAN_POINT('Ctrl Pts',(-2.48988366473036,-6.76025243720484,
-8.01416928096036));
#29750=CARTESIAN_POINT('Ctrl Pts',(-2.43063510198552,-2.12787026245138,
-10.2664546180655));
#29751=CARTESIAN_POINT('Ctrl Pts',(-2.37138653924069,3.01808597850499,-10.0408704455826));
#29752=CARTESIAN_POINT('Ctrl Pts',(-2.31213797649586,7.43560932790665,-7.39186283702356));
#29753=CARTESIAN_POINT('Ctrl Pts',(-2.25288941375102,10.0585044123173,-2.95878543764436));
#29754=CARTESIAN_POINT('Ctrl Pts',(-2.19364085100618,10.2537199985417,2.18841231721289));
#29755=CARTESIAN_POINT('Ctrl Pts',(-2.13439228826135,7.97413965087761,6.80742382307171));
#29756=CARTESIAN_POINT('Ctrl Pts',(-2.07514372551652,3.76995356138932,9.78342334888923));
#29757=CARTESIAN_POINT('Ctrl Pts',(-2.01589516277168,-1.34413310525547,
10.3981358172501));
#29758=CARTESIAN_POINT('Ctrl Pts',(-1.95664660002685,-6.1338053014481,8.50319674020009));
#29759=CARTESIAN_POINT('Ctrl Pts',(-1.89926159565089,-9.33896099596043,
4.68011416312611));
#29760=CARTESIAN_POINT('Ctrl Pts',(-1.86162611218989,-10.0616026543616,
1.50724548874808));
#29761=CARTESIAN_POINT('Ctrl Pts',(-1.84374014964383,-10.06270133709,-0.000151152320359421));
#29762=CARTESIAN_POINT('Origin',(-9.65625985035617,0.,0.));
#29763=CARTESIAN_POINT('',(-3.34374014964383,-10.0613110750442,-0.000128831358185422));
#29764=CARTESIAN_POINT('',(-3.28125985035617,-10.0619030430615,-0.000253284982714122));
#29765=CARTESIAN_POINT('',(-9.65625985035617,-10.06205,-4.69647557663214E-13));
#29766=CARTESIAN_POINT('Ctrl Pts',(-3.28125985035617,-10.0619030430615,
-0.000253284982714569));
#29767=CARTESIAN_POINT('Ctrl Pts',(-3.27613873944682,-10.0623258355878,
-0.431950106845118));
#29768=CARTESIAN_POINT('Ctrl Pts',(-3.25126810762252,-9.92988884013124,
-2.52822450542058));
#29769=CARTESIAN_POINT('Ctrl Pts',(-3.20664795488328,-8.50225392258195,
-6.13511212637845));
#29770=CARTESIAN_POINT('Ctrl Pts',(-3.14739939213844,-4.55450947899581,
-9.44374745389952));
#29771=CARTESIAN_POINT('Ctrl Pts',(-3.08815082939361,0.492492750162627,
-10.4730785091268));
#29772=CARTESIAN_POINT('Ctrl Pts',(-3.02890226664877,5.42062894282451,-8.97467015725421));
#29773=CARTESIAN_POINT('Ctrl Pts',(-2.96965370390394,9.04046429747557,-5.31017211146357));
#29774=CARTESIAN_POINT('Ctrl Pts',(-2.9104051411591,10.478330153541,-0.36403263684834));
#29775=CARTESIAN_POINT('Ctrl Pts',(-2.85115657841426,9.38718908708332,4.66996826655597));
#29776=CARTESIAN_POINT('Ctrl Pts',(-2.79190801566943,6.03039444449335,8.57684472350524));
#29777=CARTESIAN_POINT('Ctrl Pts',(-2.7326594529246,1.21812845559219,10.4136490066149));
#29778=CARTESIAN_POINT('Ctrl Pts',(-2.67341089017976,-3.88814003672063,
9.73705754435836));
#29779=CARTESIAN_POINT('Ctrl Pts',(-2.61416232743493,-8.05598294742662,
6.71036968564828));
#29780=CARTESIAN_POINT('Ctrl Pts',(-2.56677864749373,-9.83420068152227,
2.9945391385982));
#29781=CARTESIAN_POINT('Ctrl Pts',(-2.53914448846748,-10.0616829629283,
0.664906282705056));
#29782=CARTESIAN_POINT('Ctrl Pts',(-2.53125985035617,-10.0613414668576,
0.000144586642132558));
#29783=CARTESIAN_POINT('Ctrl Pts',(-3.34374014964383,-10.0613110750442,
-0.000128831358185907));
#29784=CARTESIAN_POINT('Ctrl Pts',(-3.33561461414857,-10.0616234356738,
-0.685206748448338));
#29785=CARTESIAN_POINT('Ctrl Pts',(-3.30773955773836,-9.82504498752015,
-3.03518808148316));
#29786=CARTESIAN_POINT('Ctrl Pts',(-3.26011498041321,-8.01520819574961,
-6.75902062856823));
#29787=CARTESIAN_POINT('Ctrl Pts',(-3.20086641766838,-3.82911697615253,
-9.76041932816225));
#29788=CARTESIAN_POINT('Ctrl Pts',(-3.14161785492354,1.28115426048353,-10.4060831266845));
#29789=CARTESIAN_POINT('Ctrl Pts',(-3.08236929217871,6.08221134313651,-8.54017724968541));
#29790=CARTESIAN_POINT('Ctrl Pts',(-3.02312072943387,9.41529076468844,-4.61304911040355));
#29791=CARTESIAN_POINT('Ctrl Pts',(-2.96387216668904,10.4759341041022,0.427465700532903));
#29792=CARTESIAN_POINT('Ctrl Pts',(-2.9046236039442,9.00814882168857,5.36480913779172));
#29793=CARTESIAN_POINT('Ctrl Pts',(-2.84537504119937,5.36619357179512,9.00732417694884));
#29794=CARTESIAN_POINT('Ctrl Pts',(-2.78612647845453,0.429075782469587,
10.4758682815087));
#29795=CARTESIAN_POINT('Ctrl Pts',(-2.7268779157097,-4.61160198332664,9.41599965091337));
#29796=CARTESIAN_POINT('Ctrl Pts',(-2.66762935296486,-8.5392423501426,6.08352384429894));
#29797=CARTESIAN_POINT('Ctrl Pts',(-2.62325009760957,-9.93742410704811,
2.48757824070357));
#29798=CARTESIAN_POINT('Ctrl Pts',(-2.59862036316923,-10.0623746461297,
0.411637313372905));
#29799=CARTESIAN_POINT('Ctrl Pts',(-2.59374014964383,-10.0619647730755,
0.000254798100391383));
#29800=CARTESIAN_POINT('Origin',(-9.65625985035617,0.,0.));
#29801=CARTESIAN_POINT('',(-4.09374014964383,-10.0627834482744,-0.000116052230568764));
#29802=CARTESIAN_POINT('',(-4.03125985035617,-10.0627446112277,0.000134087670397226));
#29803=CARTESIAN_POINT('',(-9.65625985035617,-10.06205,-4.69647557663214E-13));
#29804=CARTESIAN_POINT('Ctrl Pts',(-4.03125985035617,-10.0627446112277,
0.000134087670397437));
#29805=CARTESIAN_POINT('Ctrl Pts',(-4.01313299042616,-10.0617332034697,
-1.52754589633415));
#29806=CARTESIAN_POINT('Ctrl Pts',(-3.9752566095812,-9.32400657210876,-4.72060274017016));
#29807=CARTESIAN_POINT('Ctrl Pts',(-3.91763070782129,-6.08221135112264,
-8.54017726089867));
#29808=CARTESIAN_POINT('Ctrl Pts',(-3.85838214507646,-1.28115426216585,
-10.4060831403478));
#29809=CARTESIAN_POINT('Ctrl Pts',(-3.79913358233163,3.8291169811801,-9.76041934097784));
#29810=CARTESIAN_POINT('Ctrl Pts',(-3.73988501958678,8.01520820627361,-6.75902063744299));
#29811=CARTESIAN_POINT('Ctrl Pts',(-3.68063645684196,10.2667815509319,-2.12629234884133));
#29812=CARTESIAN_POINT('Ctrl Pts',(-3.62138789409711,10.0404064788223,3.01962916718597));
#29813=CARTESIAN_POINT('Ctrl Pts',(-3.56213933135229,7.39071995175672,7.43674533394825));
#29814=CARTESIAN_POINT('Ctrl Pts',(-3.50289076860744,2.95723947598601,10.0589590539462));
#29815=CARTESIAN_POINT('Ctrl Pts',(-3.44364220586262,-2.18998822827795,
10.2533835453132));
#29816=CARTESIAN_POINT('Ctrl Pts',(-3.38439364311777,-6.80864932809227,
7.97309330776734));
#29817=CARTESIAN_POINT('Ctrl Pts',(-3.3302661912823,-9.52682993830807,4.13187548496956));
#29818=CARTESIAN_POINT('Ctrl Pts',(-3.29588826036176,-10.0606953397857,
1.23288503599762));
#29819=CARTESIAN_POINT('Ctrl Pts',(-3.28125985035617,-10.0619030430615,
-0.000253284982714569));
#29820=CARTESIAN_POINT('Ctrl Pts',(-4.09374014964383,-10.0627834482744,
-0.00011605223056925));
#29821=CARTESIAN_POINT('Ctrl Pts',(-4.09235838604285,-10.0628518624021,
-0.11656583648092));
#29822=CARTESIAN_POINT('Ctrl Pts',(-4.07122710152693,-10.032574667649,-1.89739454732072));
#29823=CARTESIAN_POINT('Ctrl Pts',(-4.03034629609606,-9.04046428560539,
-5.31017210449113));
#29824=CARTESIAN_POINT('Ctrl Pts',(-3.97109773335123,-5.42062893570726,
-8.9746701454703));
#29825=CARTESIAN_POINT('Ctrl Pts',(-3.9118491706064,-0.492492749516077,
-10.4730784953755));
#29826=CARTESIAN_POINT('Ctrl Pts',(-3.85260060786156,4.5545094730156,-9.4437474414998));
#29827=CARTESIAN_POINT('Ctrl Pts',(-3.79335204511673,8.50225391141831,-6.13511211832306));
#29828=CARTESIAN_POINT('Ctrl Pts',(-3.73410348237189,10.3979291094031,-1.34573121924465));
#29829=CARTESIAN_POINT('Ctrl Pts',(-3.67485491962706,9.78400265213786,3.76844986454401));
#29830=CARTESIAN_POINT('Ctrl Pts',(-3.61560635688222,6.80864931915254,7.97309329729851));
#29831=CARTESIAN_POINT('Ctrl Pts',(-3.55635779413739,2.18998822540255,10.2533835318504));
#29832=CARTESIAN_POINT('Ctrl Pts',(-3.49710923139255,-2.95723947210302,
10.0589590407387));
#29833=CARTESIAN_POINT('Ctrl Pts',(-3.43786066864772,-7.39071994205252,
7.43674532418379));
#29834=CARTESIAN_POINT('Ctrl Pts',(-3.38673764139814,-9.67702006601549,
3.62540645957803));
#29835=CARTESIAN_POINT('Ctrl Pts',(-3.35536413506351,-10.0608642275218,
0.979909434950409));
#29836=CARTESIAN_POINT('Ctrl Pts',(-3.34374014964383,-10.0613110750442,
-0.000128831358185907));
#29837=CARTESIAN_POINT('Origin',(-9.65625985035617,0.,0.));
#29838=CARTESIAN_POINT('',(-4.84374014964383,-10.0618424730707,0.000250336541640639));
#29839=CARTESIAN_POINT('',(-4.78125985035617,-10.0612843796716,0.000112408078518301));
#29840=CARTESIAN_POINT('',(-9.65625985035617,-10.06205,-4.69647557663214E-13));
#29841=CARTESIAN_POINT('Ctrl Pts',(-4.78125985035617,-10.0612843796716,
0.000112408078517881));
#29842=CARTESIAN_POINT('Ctrl Pts',(-4.76987676232044,-10.0609038653183,
-0.959622679855897));
#29843=CARTESIAN_POINT('Ctrl Pts',(-4.73874415336977,-9.68812791873437,
-3.58477606207291));
#29844=CARTESIAN_POINT('Ctrl Pts',(-4.68786202350414,-7.43560933766978,
-7.3918628467291));
#29845=CARTESIAN_POINT('Ctrl Pts',(-4.62861346075931,-3.01808598246791,
-10.0408704587663));
#29846=CARTESIAN_POINT('Ctrl Pts',(-4.56936489801447,2.12787026524513,-10.2664546315455));
#29847=CARTESIAN_POINT('Ctrl Pts',(-4.51011633526964,6.76025244608102,-8.01416929148315));
#29848=CARTESIAN_POINT('Ctrl Pts',(-4.4508677725248,9.7610077375538,-3.82761681921153));
#29849=CARTESIAN_POINT('Ctrl Pts',(-4.39161920977998,10.4058861118699,1.28275359835361));
#29850=CARTESIAN_POINT('Ctrl Pts',(-4.33237064703513,8.53924236135476,6.08352385228661));
#29851=CARTESIAN_POINT('Ctrl Pts',(-4.2731220842903,4.61160198938182,9.41599966327665));
#29852=CARTESIAN_POINT('Ctrl Pts',(-4.21387352154547,-0.429075783032848,
10.4758682952637));
#29853=CARTESIAN_POINT('Ctrl Pts',(-4.15462495880063,-5.3661935788409,9.00732418877565));
#29854=CARTESIAN_POINT('Ctrl Pts',(-4.09537639605579,-9.00814883351634,
5.36480914483585));
#29855=CARTESIAN_POINT('Ctrl Pts',(-4.05425469324098,-10.02687110225,1.93802610770741));
#29856=CARTESIAN_POINT('Ctrl Pts',(-4.0328825113411,-10.0628351493527,0.136887321108126));
#29857=CARTESIAN_POINT('Ctrl Pts',(-4.03125985035617,-10.0627446112277,
0.000134087670397437));
#29858=CARTESIAN_POINT('Ctrl Pts',(-4.84374014964383,-10.0618424730707,
0.00025033654164057));
#29859=CARTESIAN_POINT('Ctrl Pts',(-4.8293526370222,-10.0606807693026,-1.2126019193507));
#29860=CARTESIAN_POINT('Ctrl Pts',(-4.79521560348561,-9.53967754434127,
-4.09128924672136));
#29861=CARTESIAN_POINT('Ctrl Pts',(-4.74132904903408,-6.85679662469408,
-7.93172505361893));
#29862=CARTESIAN_POINT('Ctrl Pts',(-4.68208048628925,-2.25202591260958,
-10.2399365997821));
#29863=CARTESIAN_POINT('Ctrl Pts',(-4.62283192354441,2.89628456575783,-10.0766789168245));
#29864=CARTESIAN_POINT('Ctrl Pts',(-4.56358336079958,7.34555964353492,-7.48135521158391));
#29865=CARTESIAN_POINT('Ctrl Pts',(-4.50433479805474,10.0219404799498,-3.08036220191168));
#29866=CARTESIAN_POINT('Ctrl Pts',(-4.44508623530991,10.2794667393936,2.0640944339644));
#29867=CARTESIAN_POINT('Ctrl Pts',(-4.38583767256508,8.0559829368491,6.71036967683738));
#29868=CARTESIAN_POINT('Ctrl Pts',(-4.32658910982024,3.88814003161556,9.73705753157345));
#29869=CARTESIAN_POINT('Ctrl Pts',(-4.2673405470754,-1.21812845399267,10.4136489929417));
#29870=CARTESIAN_POINT('Ctrl Pts',(-4.20809198433057,-6.03039443657531,
8.57684471224378));
#29871=CARTESIAN_POINT('Ctrl Pts',(-4.15022518518671,-9.30890368803934,
4.76108236386482));
#29872=CARTESIAN_POINT('Ctrl Pts',(-4.1121079069578,-10.061874020574,1.54784871892385));
#29873=CARTESIAN_POINT('Ctrl Pts',(-4.09374014964383,-10.0627834482744,
-0.00011605223056925));
#29874=CARTESIAN_POINT('Origin',(-9.65625985035617,0.,0.));
#29875=CARTESIAN_POINT('',(-5.59374014964383,-10.061375386696,-0.000159589291578444));
#29876=CARTESIAN_POINT('',(-5.53125985035618,-10.0620274206975,-0.000254850986975038));
#29877=CARTESIAN_POINT('',(-9.65625985035617,-10.06205,-4.69647557663214E-13));
#29878=CARTESIAN_POINT('Ctrl Pts',(-5.53125985035617,-10.0620274206975,
-0.000254850986975523));
#29879=CARTESIAN_POINT('Ctrl Pts',(-5.52662053421473,-10.0624218030828,
-0.391323674499798));
#29880=CARTESIAN_POINT('Ctrl Pts',(-5.50223169715834,-9.94483149077408,
-2.44693269826794));
#29881=CARTESIAN_POINT('Ctrl Pts',(-5.458093339187,-8.57591778746981,-6.03171258183405));
#29882=CARTESIAN_POINT('Ctrl Pts',(-5.39884477644216,-4.6685254578629,-9.38790672176614));
#29883=CARTESIAN_POINT('Ctrl Pts',(-5.33959621369733,0.365643087792113,
-10.4782740801931));
#29884=CARTESIAN_POINT('Ctrl Pts',(-5.2803476509525,5.31156151280302,-9.03964804973101));
#29885=CARTESIAN_POINT('Ctrl Pts',(-5.22109908820765,8.975503168763,-5.41924952690144));
#29886=CARTESIAN_POINT('Ctrl Pts',(-5.16185052546283,10.4731540785531,-0.490883096248158));
#29887=CARTESIAN_POINT('Ctrl Pts',(-5.10260196271799,9.44304734211565,4.55596087141438));
#29888=CARTESIAN_POINT('Ctrl Pts',(-5.04335339997316,6.13380530950194,8.50319675136485));
#29889=CARTESIAN_POINT('Ctrl Pts',(-4.98410483722832,1.34413310702038,10.3981358309029));
#29890=CARTESIAN_POINT('Ctrl Pts',(-4.92485627448348,-3.76995356633927,
9.78342336173498));
#29891=CARTESIAN_POINT('Ctrl Pts',(-4.86560771173865,-7.97413966134769,
6.80742383201003));
#29892=CARTESIAN_POINT('Ctrl Pts',(-4.81774223702955,-9.81575725621947,
3.07583662613618));
#29893=CARTESIAN_POINT('Ctrl Pts',(-4.78962628323539,-10.0615640531474,
0.705506161498075));
#29894=CARTESIAN_POINT('Ctrl Pts',(-4.78125985035617,-10.0612843796716,
0.000112408078517881));
#29895=CARTESIAN_POINT('Ctrl Pts',(-5.59374014964383,-10.061375386696,-0.000159589291578652));
#29896=CARTESIAN_POINT('Ctrl Pts',(-5.58609640891648,-10.0617424196366,
-0.64460476064184));
#29897=CARTESIAN_POINT('Ctrl Pts',(-5.55870314727419,-9.84322461794499,
-2.95388988874244));
#29898=CARTESIAN_POINT('Ctrl Pts',(-5.51156036471693,-8.09646237954581,
-6.66147275121817));
#29899=CARTESIAN_POINT('Ctrl Pts',(-5.4523118019721,-3.94702056424182,-9.71333881546786));
#29900=CARTESIAN_POINT('Ctrl Pts',(-5.39306323922727,1.15505799604341,-10.420833138689));
#29901=CARTESIAN_POINT('Ctrl Pts',(-5.33381467648243,5.97835648115395,-8.61319778380056));
#29902=CARTESIAN_POINT('Ctrl Pts',(-5.27456611373759,9.35874329001436,-4.72671622907851));
#29903=CARTESIAN_POINT('Ctrl Pts',(-5.21531755099276,10.480342084015,0.300586228304444));
#29904=CARTESIAN_POINT('Ctrl Pts',(-5.15606898824793,9.07244836417983,5.25534042264758));
#29905=CARTESIAN_POINT('Ctrl Pts',(-5.09682042550309,5.47486560219418,8.9416871403854));
#29906=CARTESIAN_POINT('Ctrl Pts',(-5.03757186275826,0.555891663852748,
10.4699048102971));
#29907=CARTESIAN_POINT('Ctrl Pts',(-4.97832330001342,-4.49725001357077,
9.47114906408194));
#29908=CARTESIAN_POINT('Ctrl Pts',(-4.91907473726859,-8.464953815877,6.18647550497794));
#29909=CARTESIAN_POINT('Ctrl Pts',(-4.87421368714539,-9.92222535333499,
2.5688714186231));
#29910=CARTESIAN_POINT('Ctrl Pts',(-4.84910215793714,-10.0622754224904,
0.452262023737051));
#29911=CARTESIAN_POINT('Ctrl Pts',(-4.84374014964383,-10.0618424730707,
0.00025033654164057));
#29912=CARTESIAN_POINT('Origin',(-9.65625985035617,0.,0.));
#29913=CARTESIAN_POINT('',(-6.34374014964383,-10.0628459703277,-7.75181276524428E-5));
#29914=CARTESIAN_POINT('',(-6.28125985035617,-10.0626541504143,0.000167148211893109));
#29915=CARTESIAN_POINT('',(-9.65625985035617,-10.06205,-4.69647557663214E-13));
#29916=CARTESIAN_POINT('Ctrl Pts',(-6.28125985035617,-10.0626541504143,
0.000167148211892981));
#29917=CARTESIAN_POINT('Ctrl Pts',(-6.26361478519406,-10.0614821172421,
-1.48694732055795));
#29918=CARTESIAN_POINT('Ctrl Pts',(-6.22622019911701,-9.35376745039498,
-4.63961696798018));
#29919=CARTESIAN_POINT('Ctrl Pts',(-6.16907609212502,-6.18517442841409,
-8.46590455045353));
#29920=CARTESIAN_POINT('Ctrl Pts',(-6.10982752938018,-1.40706268161673,
-10.3898073695953));
#29921=CARTESIAN_POINT('Ctrl Pts',(-6.05057896663535,3.71065196087965,-9.80606876339935));
#29922=CARTESIAN_POINT('Ctrl Pts',(-5.99133040389051,7.93277881804871,-6.85557749509213));
#29923=CARTESIAN_POINT('Ctrl Pts',(-5.93208184114569,10.2402826148908,-2.25045207335339));
#29924=CARTESIAN_POINT('Ctrl Pts',(-5.87283327840083,10.0762336698203,2.89783325926043));
#29925=CARTESIAN_POINT('Ctrl Pts',(-5.81358471565602,7.4802261654632,7.34670940495238));
#29926=CARTESIAN_POINT('Ctrl Pts',(-5.75433615291117,3.07882185862981,10.0224138075675));
#29927=CARTESIAN_POINT('Ctrl Pts',(-5.69508759016634,-2.06567430345103,
10.2791493927931));
#29928=CARTESIAN_POINT('Ctrl Pts',(-5.63583902742151,-6.7116077616892,8.05495150950825));
#29929=CARTESIAN_POINT('Ctrl Pts',(-5.58122978081811,-9.50070766399809,
4.21303279626446));
#29930=CARTESIAN_POINT('Ctrl Pts',(-5.54637005512967,-10.0607429213405,
1.27345226955577));
#29931=CARTESIAN_POINT('Ctrl Pts',(-5.53125985035617,-10.0620274206975,
-0.000254850986975523));
#29932=CARTESIAN_POINT('Ctrl Pts',(-6.34374014964383,-10.0628459703277,
-7.75181276522433E-5));
#29933=CARTESIAN_POINT('Ctrl Pts',(-6.34284018081076,-10.0628773940367,
-0.0759221005433881));
#29934=CARTESIAN_POINT('Ctrl Pts',(-6.32219069106275,-10.0436093238266,
-1.81613516389724));
#29935=CARTESIAN_POINT('Ctrl Pts',(-6.28179168039979,-9.10409988500852,
-5.20031610215367));
#29936=CARTESIAN_POINT('Ctrl Pts',(-6.22254311765495,-5.52890158316907,
-8.90837637071521));
#29937=CARTESIAN_POINT('Ctrl Pts',(-6.16329455491012,-0.61927020154201,
-10.4663473426058));
#29938=CARTESIAN_POINT('Ctrl Pts',(-6.10404599216529,4.43982570388255,-9.49820351423256));
#29939=CARTESIAN_POINT('Ctrl Pts',(-6.04479742942044,8.42734343078316,-6.23761212149772));
#29940=CARTESIAN_POINT('Ctrl Pts',(-5.98554886667563,10.3808720045808,-1.47153617119417));
#29941=CARTESIAN_POINT('Ctrl Pts',(-5.92630030393077,9.82891575620613,3.64970373263731));
#29942=CARTESIAN_POINT('Ctrl Pts',(-5.86705174118595,6.90469258895211,7.89006606630713));
#29943=CARTESIAN_POINT('Ctrl Pts',(-5.80780317844112,2.31398105003217,10.2261143147686));
#29944=CARTESIAN_POINT('Ctrl Pts',(-5.74855461569627,-2.83522349381956,
10.094029424304));
#29945=CARTESIAN_POINT('Ctrl Pts',(-5.68930605295145,-7.3001300877402,7.5256908640133));
#29946=CARTESIAN_POINT('Ctrl Pts',(-5.63770123093395,-9.65439224755071,
3.70665976616409));
#29947=CARTESIAN_POINT('Ctrl Pts',(-5.60584592983142,-10.0607940979973,
1.020480940731));
#29948=CARTESIAN_POINT('Ctrl Pts',(-5.59374014964383,-10.061375386696,-0.000159589291578652));
#29949=CARTESIAN_POINT('Origin',(-9.65625985035617,0.,0.));
#29950=CARTESIAN_POINT('',(-7.09374014964383,-10.0617260250247,0.000240284390234935));
#29951=CARTESIAN_POINT('',(-7.03125985035617,-10.0612423609455,7.79087254440521E-5));
#29952=CARTESIAN_POINT('',(-9.65625985035617,-10.06205,-4.69647557663214E-13));
#29953=CARTESIAN_POINT('Ctrl Pts',(-7.03125985035617,-10.0612423609455,
7.79087254439148E-5));
#29954=CARTESIAN_POINT('Ctrl Pts',(-7.02035855708835,-10.0609911152643,
-0.919046910462609));
#29955=CARTESIAN_POINT('Ctrl Pts',(-6.98970774290558,-9.70993335321315,
-3.50350861223781));
#29956=CARTESIAN_POINT('Ctrl Pts',(-6.93930740780787,-7.52456879985629,
-7.30128666317293));
#29957=CARTESIAN_POINT('Ctrl Pts',(-6.88005884506304,-3.13944487805482,
-10.0035897771931));
#29958=CARTESIAN_POINT('Ctrl Pts',(-6.8208102823182,2.0034026226881,-10.2914673635639));
#29959=CARTESIAN_POINT('Ctrl Pts',(-6.76156171957337,6.6627170580516,-8.09543846701894));
#29960=CARTESIAN_POINT('Ctrl Pts',(-6.70231315682853,9.71394534640064,-3.94552764200815));
#29961=CARTESIAN_POINT('Ctrl Pts',(-6.6430645940837,10.4206555039509,1.1566596022022));
#29962=CARTESIAN_POINT('Ctrl Pts',(-6.58381603133886,8.61227885655681,5.97968021421488));
#29963=CARTESIAN_POINT('Ctrl Pts',(-6.52456746859403,4.72527779786631,9.35946965913116));
#29964=CARTESIAN_POINT('Ctrl Pts',(-6.46531890584919,-0.302196989616849,
10.480295775732));
#29965=CARTESIAN_POINT('Ctrl Pts',(-6.40607034310435,-5.25673474729183,
9.07164055526217));
#29966=CARTESIAN_POINT('Ctrl Pts',(-6.34682178035952,-8.94252849986846,
5.4734912621059));
#29967=CARTESIAN_POINT('Ctrl Pts',(-6.30521828277679,-10.015090324262,2.01929287385976));
#29968=CARTESIAN_POINT('Ctrl Pts',(-6.28336430610901,-10.0627939340835,
0.177529292821701));
#29969=CARTESIAN_POINT('Ctrl Pts',(-6.28125985035617,-10.0626541504143,
0.000167148211892981));
#29970=CARTESIAN_POINT('Ctrl Pts',(-7.09374014964383,-10.0617260250247,
0.00024028439023438));
#29971=CARTESIAN_POINT('Ctrl Pts',(-7.0798344317901,-10.0606687753925,-1.17203615203383));
#29972=CARTESIAN_POINT('Ctrl Pts',(-7.04617919302143,-9.56494781223263,
-4.01010281132586));
#29973=CARTESIAN_POINT('Ctrl Pts',(-6.9927744333378,-6.95233545178506,-7.84811784659899));
#29974=CARTESIAN_POINT('Ctrl Pts',(-6.93352587059297,-2.37585136897494,
-10.2119171916642));
#29975=CARTESIAN_POINT('Ctrl Pts',(-6.87427730784814,2.77405849573116,-10.1110099229398));
#29976=CARTESIAN_POINT('Ctrl Pts',(-6.8150287451033,7.25443293930229,-7.56975065851036));
#29977=CARTESIAN_POINT('Ctrl Pts',(-6.75578018235847,9.98390711286757,-3.20148731676458));
#29978=CARTESIAN_POINT('Ctrl Pts',(-6.69653161961363,10.3037062860758,1.93947390886785));
#29979=CARTESIAN_POINT('Ctrl Pts',(-6.63728305686881,8.13664504012033,6.61233164437115));
#29980=CARTESIAN_POINT('Ctrl Pts',(-6.57803449412396,4.00575641567419,9.68926404911563));
#29981=CARTESIAN_POINT('Ctrl Pts',(-6.51878593137913,-1.09194519850991,
10.4276353006677));
#29982=CARTESIAN_POINT('Ctrl Pts',(-6.45953736863429,-5.92609938437677,
8.64923513176283));
#29983=CARTESIAN_POINT('Ctrl Pts',(-6.40118877472253,-9.27825086183916,
4.84201353009798));
#29984=CARTESIAN_POINT('Ctrl Pts',(-6.3625897017257,-10.0621878110463,1.58846238885859));
#29985=CARTESIAN_POINT('Ctrl Pts',(-6.34374014964383,-10.0628459703277,
-7.75181276522433E-5));
#29986=CARTESIAN_POINT('Origin',(-9.65625985035617,0.,0.));
#29987=CARTESIAN_POINT('',(-7.84374014964383,-10.0614619079128,-0.000218150500570502));
#29988=CARTESIAN_POINT('',(-7.78125985035617,-10.0621541710632,-0.000250329009834688));
#29989=CARTESIAN_POINT('',(-9.65625985035617,-10.06205,-4.69647557663214E-13));
#29990=CARTESIAN_POINT('',(-8.,-2.60344811511687,9.71940883564398));
#29991=CARTESIAN_POINT('Ctrl Pts',(-8.,-2.60344811511687,9.71940883564398));
#29992=CARTESIAN_POINT('Ctrl Pts',(-7.98025047908506,-4.2115554043733,9.28866001522532));
#29993=CARTESIAN_POINT('Ctrl Pts',(-7.94075143725516,-7.20829614504029,
7.61418486945486));
#29994=CARTESIAN_POINT('Ctrl Pts',(-7.88866482046978,-9.63126793254245,
3.78770677709999));
#29995=CARTESIAN_POINT('Ctrl Pts',(-7.85632772459933,-10.0607601076051,
1.06096981025071));
#29996=CARTESIAN_POINT('Ctrl Pts',(-7.84374014964383,-10.0614619079128,
-0.000218150500570363));
#29997=CARTESIAN_POINT('',(-8.,2.6037558201701,9.72001092048762));
#29998=CARTESIAN_POINT('Origin',(-8.,0.,0.));
#29999=CARTESIAN_POINT('Ctrl Pts',(-8.,2.6037558201701,9.72001092048762));
#30000=CARTESIAN_POINT('Ctrl Pts',(-7.98217765815669,1.15257245541084,10.107573988037));
#30001=CARTESIAN_POINT('Ctrl Pts',(-7.94460579539843,-2.09302813938078,
10.2328568518709));
#30002=CARTESIAN_POINT('Ctrl Pts',(-7.88728441172523,-6.61358902169624,
8.13565037958078));
#30003=CARTESIAN_POINT('Ctrl Pts',(-7.83219337035393,-9.47401039595774,
4.29415937030418));
#30004=CARTESIAN_POINT('Ctrl Pts',(-7.79685184989758,-10.0608163520868,
1.3140197112117));
#30005=CARTESIAN_POINT('Ctrl Pts',(-7.78125985035617,-10.0621541710632,
-0.000250329009834835));
#30006=CARTESIAN_POINT('Origin',(-9.65625985035617,0.,0.));
#30007=CARTESIAN_POINT('Ctrl Pts',(-7.78125985035617,-10.0621541710632,
-0.000250329009834835));
#30008=CARTESIAN_POINT('Ctrl Pts',(-7.77710232898263,-10.062510893174,-0.350693244834193));
#30009=CARTESIAN_POINT('Ctrl Pts',(-7.75319528669415,-9.95926473270352,
-2.36564048511104));
#30010=CARTESIAN_POINT('Ctrl Pts',(-7.70953872349072,-8.64832327843871,
-5.92743166991522));
#30011=CARTESIAN_POINT('Ctrl Pts',(-7.65029016074589,-4.78185742483636,
-9.33068795739798));
#30012=CARTESIAN_POINT('Ctrl Pts',(-7.59104159800105,0.238740070891225,
-10.4819341157898));
#30013=CARTESIAN_POINT('Ctrl Pts',(-7.53179303525622,5.20171515908679,-9.10330011423497));
#30014=CARTESIAN_POINT('Ctrl Pts',(-7.47254447251139,8.90922610438627,-5.52753257885261));
#30015=CARTESIAN_POINT('Ctrl Pts',(-7.41329590976654,10.4664423751253,-0.617661469275298));
#30016=CARTESIAN_POINT('Ctrl Pts',(-7.35404734702172,9.49752105893024,4.4412854149463));
#30017=CARTESIAN_POINT('Ctrl Pts',(-7.29479878427687,6.23631681532395,8.42830205522834));
#30018=CARTESIAN_POINT('Ctrl Pts',(-7.23555022153205,1.46994068417205,10.38109804613));
#30019=CARTESIAN_POINT('Ctrl Pts',(-7.17630165878721,-3.65121434111183,
9.82835472395443));
#30020=CARTESIAN_POINT('Ctrl Pts',(-7.11705309604238,-7.89112719116351,
6.90347985740062));
#30021=CARTESIAN_POINT('Ctrl Pts',(-7.06870582656536,-9.79678423589676,
3.15713204118938));
#30022=CARTESIAN_POINT('Ctrl Pts',(-7.0401080780033,-10.06144628895,0.746101837858744));
#30023=CARTESIAN_POINT('Ctrl Pts',(-7.03125985035617,-10.0612423609455,
7.79087254439148E-5));
#30024=CARTESIAN_POINT('Ctrl Pts',(-7.84374014964383,-10.0614619079128,
-0.000218150500570363));
#30025=CARTESIAN_POINT('Ctrl Pts',(-7.83657820368438,-10.0618612108679,
-0.60400171124062));
#30026=CARTESIAN_POINT('Ctrl Pts',(-7.80966673680999,-9.86084825550603,
-2.87248335114659));
#30027=CARTESIAN_POINT('Ctrl Pts',(-7.76300574902067,-8.17655263057037,
-6.56303005806257));
#30028=CARTESIAN_POINT('Ctrl Pts',(-7.70375718627582,-4.06433342707358,
-9.66479172255802));
#30029=CARTESIAN_POINT('Ctrl Pts',(-7.644508623531,1.02878615653537,-10.4340771844272));
#30030=CARTESIAN_POINT('Ctrl Pts',(-7.58526006078616,5.87362828262073,-8.68494406353048));
#30031=CARTESIAN_POINT('Ctrl Pts',(-7.52601149804132,9.30082195115954,-4.83969619824767));
#30032=CARTESIAN_POINT('Ctrl Pts',(-7.46676293529649,10.483214281353,0.173665734501785));
#30033=CARTESIAN_POINT('Ctrl Pts',(-7.40751437255165,9.13541724029078,5.1450995797055));
#30034=CARTESIAN_POINT('Ctrl Pts',(-7.34826580980682,5.58273512973762,8.87473987601911));
#30035=CARTESIAN_POINT('Ctrl Pts',(-7.28901724706198,0.682625919309218,
10.4624057987323));
#30036=CARTESIAN_POINT('Ctrl Pts',(-7.22976868431715,-4.38223858668436,
9.52491001985317));
#30037=CARTESIAN_POINT('Ctrl Pts',(-7.17052012157231,-8.38942416699272,
6.28851997968158));
#30038=CARTESIAN_POINT('Ctrl Pts',(-7.1251772766812,-9.90651266144331,2.65016697566111));
#30039=CARTESIAN_POINT('Ctrl Pts',(-7.09958395270504,-10.0621703284905,
0.49288314539355));
#30040=CARTESIAN_POINT('Ctrl Pts',(-7.09374014964383,-10.0617260250247,
0.00024028439023438));
#30041=CARTESIAN_POINT('Ctrl Pts',(-8.,7.21801009705396,-6.39216838336781));
#30042=CARTESIAN_POINT('Ctrl Pts',(-7.98025047908506,8.27561480792393,-5.19792551867511));
#30043=CARTESIAN_POINT('Ctrl Pts',(-7.94075143725517,9.78570906708942,-2.27567127227239));
#30044=CARTESIAN_POINT('Ctrl Pts',(-7.88150287451033,9.68796046702948,2.65991246200497));
#30045=CARTESIAN_POINT('Ctrl Pts',(-7.8222543117655,7.25238499100985,6.95222960735294));
#30046=CARTESIAN_POINT('Ctrl Pts',(-7.76300574902066,3.06619992068337,9.56722174110869));
#30047=CARTESIAN_POINT('Ctrl Pts',(-7.70375718627582,-1.85992661552226,
9.87278141350118));
#30048=CARTESIAN_POINT('Ctrl Pts',(-7.64450862353099,-6.33720258119721,
7.79565594657622));
#30049=CARTESIAN_POINT('Ctrl Pts',(-7.58526006078615,-9.28492944394566,
3.83691534180259));
#30050=CARTESIAN_POINT('Ctrl Pts',(-7.52601149804132,-9.99169809387859,
-1.04784215725893));
#30051=CARTESIAN_POINT('Ctrl Pts',(-7.46676293529649,-8.28690389187399,
-5.67972021775593));
#30052=CARTESIAN_POINT('Ctrl Pts',(-7.40751437255165,-4.58202030942313,
-8.94075208090305));
#30053=CARTESIAN_POINT('Ctrl Pts',(-7.34826580980682,0.228762958890216,
-10.0438868693848));
#30054=CARTESIAN_POINT('Ctrl Pts',(-7.28901724706198,4.98433189977125,-8.72286693232514));
#30055=CARTESIAN_POINT('Ctrl Pts',(-7.22976868431715,8.53690340902155,-5.29653318514979));
#30056=CARTESIAN_POINT('Ctrl Pts',(-7.17052012157231,10.0290425392331,-0.591848971043799));
#30057=CARTESIAN_POINT('Ctrl Pts',(-7.11127155882747,9.10061311221161,4.25568103840426));
#30058=CARTESIAN_POINT('Ctrl Pts',(-7.05202299608264,5.97569684018532,8.07607750712695));
#30059=CARTESIAN_POINT('Ctrl Pts',(-6.99277443333781,1.40851085052043,9.94726480852957));
#30060=CARTESIAN_POINT('Ctrl Pts',(-6.93352587059297,-3.49862757892743,
9.4176210105041));
#30061=CARTESIAN_POINT('Ctrl Pts',(-6.87427730784813,-7.56135155062463,
6.61497867920762));
#30062=CARTESIAN_POINT('Ctrl Pts',(-6.8150287451033,-9.79909863393696,2.21577215777723));
#30063=CARTESIAN_POINT('Ctrl Pts',(-6.75578018235847,-9.67177533431446,
-2.71822408062585));
#30064=CARTESIAN_POINT('Ctrl Pts',(-6.69653161961363,-7.21011188696681,
-6.99616086456685));
#30065=CARTESIAN_POINT('Ctrl Pts',(-6.6372830568688,-3.00824531422618,-9.58553287017026));
#30066=CARTESIAN_POINT('Ctrl Pts',(-6.57803449412396,1.91967904719004,-9.8613798539234));
#30067=CARTESIAN_POINT('Ctrl Pts',(-6.51878593137913,6.38427752307505,-7.75712451753733));
#30068=CARTESIAN_POINT('Ctrl Pts',(-6.45953736863429,9.30799287964075,-3.78064132426331));
#30069=CARTESIAN_POINT('Ctrl Pts',(-6.40028880588946,9.98516913294189,1.10832200074663));
#30070=CARTESIAN_POINT('Ctrl Pts',(-6.34104024314462,8.2523657912091,5.72978525940176));
#30071=CARTESIAN_POINT('Ctrl Pts',(-6.28179168039979,4.52780518403485,8.96833097549665));
#30072=CARTESIAN_POINT('Ctrl Pts',(-6.22254311765496,-0.289567969274681,
10.0423169966864));
#30073=CARTESIAN_POINT('Ctrl Pts',(-6.16329455491011,-5.03705218148902,
8.69253044812817));
#30074=CARTESIAN_POINT('Ctrl Pts',(-6.10404599216529,-8.56881407445866,
5.24475029225229));
#30075=CARTESIAN_POINT('Ctrl Pts',(-6.04479742942045,-10.0324420382062,
0.531118650339597));
#30076=CARTESIAN_POINT('Ctrl Pts',(-5.98554886667561,-9.07468081182084,
-4.31070161740279));
#30077=CARTESIAN_POINT('Ctrl Pts',(-5.92630030393079,-5.92669172885007,
-8.11210856817701));
#30078=CARTESIAN_POINT('Ctrl Pts',(-5.86705174118593,-1.34826056300076,
-9.95561016336843));
#30079=CARTESIAN_POINT('Ctrl Pts',(-5.80780317844112,3.55558125962594,-9.39626639559069));
#30080=CARTESIAN_POINT('Ctrl Pts',(-5.74855461569627,7.60126252733364,-6.56907818961398));
#30081=CARTESIAN_POINT('Ctrl Pts',(-5.68930605295145,9.81233415115218,-2.15640413115026));
#30082=CARTESIAN_POINT('Ctrl Pts',(-5.6300574902066,9.65514092448912,2.77673081139753));
#30083=CARTESIAN_POINT('Ctrl Pts',(-5.57080892746178,7.16762236180716,7.03968535868123));
#30084=CARTESIAN_POINT('Ctrl Pts',(-5.51156036471693,2.95015577253862,9.60357023134971));
#30085=CARTESIAN_POINT('Ctrl Pts',(-5.45231180197211,-1.97934835152263,
9.84957665963537));
#30086=CARTESIAN_POINT('Ctrl Pts',(-5.39306323922727,-6.43112505053289,
7.71832953786746));
#30087=CARTESIAN_POINT('Ctrl Pts',(-5.33381467648243,-9.33071170264792,
3.72421795720638));
#30088=CARTESIAN_POINT('Ctrl Pts',(-5.27456611373759,-9.97827592921563,
-1.16875564218737));
#30089=CARTESIAN_POINT('Ctrl Pts',(-5.21531755099277,-8.21752427624387,
-5.77964315853947));
#30090=CARTESIAN_POINT('Ctrl Pts',(-5.15606898824792,-4.47342456340985,
-8.99557963369734));
#30091=CARTESIAN_POINT('Ctrl Pts',(-5.0968204255031,0.350362611307043,-10.0403797891966));
#30092=CARTESIAN_POINT('Ctrl Pts',(-5.03757186275825,5.08958769870612,-8.66187493143883));
#30093=CARTESIAN_POINT('Ctrl Pts',(-4.97832330001343,8.60041070922793,-5.19277535652244));
#30094=CARTESIAN_POINT('Ctrl Pts',(-4.91907473726859,10.0354737559517,-0.470368753547383));
#30095=CARTESIAN_POINT('Ctrl Pts',(-4.85982617452376,9.0484158895429,4.36556412856081));
#30096=CARTESIAN_POINT('Ctrl Pts',(-4.80057761177892,5.87746936079909,8.14784230232624));
#30097=CARTESIAN_POINT('Ctrl Pts',(-4.74132904903409,1.28796085867118,9.96359057254162));
#30098=CARTESIAN_POINT('Ctrl Pts',(-4.68208048628925,-3.61240461014787,
9.37456736085946));
#30099=CARTESIAN_POINT('Ctrl Pts',(-4.62283192354442,-7.64089487250279,
6.52293690127919));
#30100=CARTESIAN_POINT('Ctrl Pts',(-4.56358336079958,-9.8252099901855,2.0969570619038));
#30101=CARTESIAN_POINT('Ctrl Pts',(-4.50433479805475,-9.63815259752371,
-2.83513575998683));
#30102=CARTESIAN_POINT('Ctrl Pts',(-4.4450862353099,-7.12487010197824,-7.08295180702551));
#30103=CARTESIAN_POINT('Ctrl Pts',(-4.38583767256508,-2.89195809047495,
-9.62125556638245));
#30104=CARTESIAN_POINT('Ctrl Pts',(-4.32658910982023,2.03894510123426,-9.83741242120418));
#30105=CARTESIAN_POINT('Ctrl Pts',(-4.26734054707541,6.47773684005869,-7.67925163682345));
#30106=CARTESIAN_POINT('Ctrl Pts',(-4.20809198433056,9.35308850105216,-3.66765807596552));
#30107=CARTESIAN_POINT('Ctrl Pts',(-4.14884342158574,9.97101696392875,1.22914644194833));
#30108=CARTESIAN_POINT('Ctrl Pts',(-4.08959485884089,8.18238154144732,5.82928920031346));
#30109=CARTESIAN_POINT('Ctrl Pts',(-4.03034629609607,4.41887996588413,9.02249855183238));
#30110=CARTESIAN_POINT('Ctrl Pts',(-3.97109773335123,-0.411144410522746,
10.0380745436764));
#30111=CARTESIAN_POINT('Ctrl Pts',(-3.9118491706064,-5.14193665307501,8.63090190689669));
#30112=CARTESIAN_POINT('Ctrl Pts',(-3.85260060786156,-8.63169208916567,
5.14061007552062));
#30113=CARTESIAN_POINT('Ctrl Pts',(-3.79335204511673,-10.0381376154984,
0.409601615017363));
#30114=CARTESIAN_POINT('Ctrl Pts',(-3.73410348237189,-9.02181929045025,
-4.42026661652537));
#30115=CARTESIAN_POINT('Ctrl Pts',(-3.67485491962706,-5.82803154947716,
-8.18327737089536));
#30116=CARTESIAN_POINT('Ctrl Pts',(-3.61560635688222,-1.22761394312144,
-9.97120575845082));
#30117=CARTESIAN_POINT('Ctrl Pts',(-3.55635779413739,3.66909554513215,-9.35252469397438));
#30118=CARTESIAN_POINT('Ctrl Pts',(-3.49710923139255,7.68024713464924,-6.47655650955208));
#30119=CARTESIAN_POINT('Ctrl Pts',(-3.43786066864772,9.83772567840422,-2.0374331270438));
#30120=CARTESIAN_POINT('Ctrl Pts',(-3.37861210590288,9.6208109764798,2.89343678444073));
#30121=CARTESIAN_POINT('Ctrl Pts',(-3.31936354315805,7.08185667442123,7.12595862418978));
#30122=CARTESIAN_POINT('Ctrl Pts',(-3.26011498041321,2.83365440140854,9.63858822671076));
#30123=CARTESIAN_POINT('Ctrl Pts',(-3.20086641766838,-2.09846711180656,
9.82488758466862));
#30124=CARTESIAN_POINT('Ctrl Pts',(-3.14161785492354,-6.52411118303607,
7.63989224675928));
#30125=CARTESIAN_POINT('Ctrl Pts',(-3.08236929217871,-9.37512245462701,
3.61096375382772));
#30126=CARTESIAN_POINT('Ctrl Pts',(-3.02312072943387,-9.96339250315773,
-1.28949218637783));
#30127=CARTESIAN_POINT('Ctrl Pts',(-2.96387216668905,-8.14693887500758,
-5.87872156489823));
#30128=CARTESIAN_POINT('Ctrl Pts',(-2.9046236039442,-4.3641733908311,-9.04908674317308));
#30129=CARTESIAN_POINT('Ctrl Pts',(-2.84537504119937,0.471911138916074,
-10.0354013446237));
#30130=CARTESIAN_POINT('Ctrl Pts',(-2.78612647845453,5.19409712570397,-8.59961250984385));
#30131=CARTESIAN_POINT('Ctrl Pts',(-2.7268779157097,8.66265706762792,-5.08825636140564));
#30132=CARTESIAN_POINT('Ctrl Pts',(-2.66762935296487,10.0404335192006,-0.348819462217449));
#30133=CARTESIAN_POINT('Ctrl Pts',(-2.60838079022003,8.99489198946221,4.47480707613385));
#30134=CARTESIAN_POINT('Ctrl Pts',(-2.54913222747519,5.77838010706614,8.21841247498393));
#30135=CARTESIAN_POINT('Ctrl Pts',(-2.48988366473036,1.16722202841516,9.97845544195549));
#30136=CARTESIAN_POINT('Ctrl Pts',(-2.43063510198552,-3.72565198652797,
9.33013920292668));
#30137=CARTESIAN_POINT('Ctrl Pts',(-2.37138653924069,-7.71931787128481,
6.42993871454248));
#30138=CARTESIAN_POINT('Ctrl Pts',(-2.31213797649585,-9.8498807570359,1.97783450846704));
#30139=CARTESIAN_POINT('Ctrl Pts',(-2.25288941375102,-9.60311669702822,
-2.95163174768923));
#30140=CARTESIAN_POINT('Ctrl Pts',(-2.19364085100618,-7.03858365582718,
-7.16870423372533));
#30141=CARTESIAN_POINT('Ctrl Pts',(-2.13439228826135,-2.77524684250714,
-9.65556757699222));
#30142=CARTESIAN_POINT('Ctrl Pts',(-2.07514372551651,2.15791220141318,-9.8120026091365));
#30143=CARTESIAN_POINT('Ctrl Pts',(-2.01589516277168,6.57024637957694,-7.60025281042448));
#30144=CARTESIAN_POINT('Ctrl Pts',(-1.95664660002684,9.39681275570056,-3.554137068968));
#30145=CARTESIAN_POINT('Ctrl Pts',(-1.89739803728201,9.95540282638318,1.34979066345517));
#30146=CARTESIAN_POINT('Ctrl Pts',(-1.83814947453718,8.11119757610343,5.92793844031152));
#30147=CARTESIAN_POINT('Ctrl Pts',(-1.77890091179234,4.30930684356341,9.07534323310842));
#30148=CARTESIAN_POINT('Ctrl Pts',(-1.71965234904751,-0.532660569034724,
10.0323602900267));
#30149=CARTESIAN_POINT('Ctrl Pts',(-1.66040378630267,-5.24606720460977,
8.56800788721785));
#30150=CARTESIAN_POINT('Ctrl Pts',(-1.60115522355784,-8.6933045095691,5.03571613324405));
#30151=CARTESIAN_POINT('Ctrl Pts',(-1.541906660813,-10.0423613829002,0.288024523165256));
#30152=CARTESIAN_POINT('Ctrl Pts',(-1.48265809806817,-8.96763497362019,
-4.52918350816273));
#30153=CARTESIAN_POINT('Ctrl Pts',(-1.42340953532333,-5.72851685357889,
-8.25324632668694));
#30154=CARTESIAN_POINT('Ctrl Pts',(-1.3641609725785,-1.10678732826568,-9.98533935731279));
#30155=CARTESIAN_POINT('Ctrl Pts',(-1.30491240983366,3.78207186121437,-9.3074117082742));
#30156=CARTESIAN_POINT('Ctrl Pts',(-1.24566384708883,7.75810565024088,-6.38308522506237));
#30157=CARTESIAN_POINT('Ctrl Pts',(-1.18641528434399,9.86167478052657,-1.91816339080776));
#30158=CARTESIAN_POINT('Ctrl Pts',(-1.12716672159916,9.58507040776671,3.00971851655006));
#30159=CARTESIAN_POINT('Ctrl Pts',(-1.06791815885432,6.99505263240274,7.21118706875814));
#30160=CARTESIAN_POINT('Ctrl Pts',(-1.00866959610949,2.71673755474579,9.67219299483537));
#30161=CARTESIAN_POINT('Ctrl Pts',(-0.949421033364656,-2.21727819104757,
9.79875796691677));
#30162=CARTESIAN_POINT('Ctrl Pts',(-0.890172470619816,-6.61614073855928,
7.56033478083375));
#30163=CARTESIAN_POINT('Ctrl Pts',(-0.830923907874984,-9.41815860919774,
3.49718010441341));
#30164=CARTESIAN_POINT('Ctrl Pts',(-0.771675345130147,-9.94704822647297,
-1.41003966289232));
#30165=CARTESIAN_POINT('Ctrl Pts',(-0.712426782385315,-8.07515895486045,
-5.9769380224696));
#30166=CARTESIAN_POINT('Ctrl Pts',(-0.653178219640479,-4.25428233525734,
-9.1012670591868));
#30167=CARTESIAN_POINT('Ctrl Pts',(-0.593929656895646,0.593390474060013,
-10.0289514913561));
#30168=CARTESIAN_POINT('Ctrl Pts',(-0.534681094150809,5.29784498478896,
-8.53608919751393));
#30169=CARTESIAN_POINT('Ctrl Pts',(-0.475432531405974,8.72363329158144,
-4.98299131693383));
#30170=CARTESIAN_POINT('Ctrl Pts',(-0.416183968661139,10.0439211359327,
-0.227219026357994));
#30171=CARTESIAN_POINT('Ctrl Pts',(-0.356935405916306,8.94004924204562,
4.58339391942193));
#30172=CARTESIAN_POINT('Ctrl Pts',(-0.297686843171469,5.67844361680366,
8.28777764910186));
#30173=CARTESIAN_POINT('Ctrl Pts',(-0.238438280426636,1.04631205793237,
9.99185725226522));
#30174=CARTESIAN_POINT('Ctrl Pts',(-0.179189717681799,-3.83835310103361,
9.28434304296069));
#30175=CARTESIAN_POINT('Ctrl Pts',(-0.119941154936966,-7.79660904980335,
6.335997758854));
#30176=CARTESIAN_POINT('Ctrl Pts',(-0.0606925921921299,-9.87310731639768,
1.8584219607967));
#30177=CARTESIAN_POINT('Ctrl Pts',(-0.00144402944729562,-9.56667277050388,
-3.06769496072332));
#30178=CARTESIAN_POINT('Ctrl Pts',(0.0578045332975387,-6.95126519921767,
-7.25340557413907));
#30179=CARTESIAN_POINT('Ctrl Pts',(0.117053096042374,-2.65812868397592,
-9.68846386678141));
#30180=CARTESIAN_POINT('Ctrl Pts',(0.176301658787208,2.27656290681844,-9.78515415130587));
#30181=CARTESIAN_POINT('Ctrl Pts',(0.235550221532044,6.6617925734103,-7.52013960614428));
#30182=CARTESIAN_POINT('Ctrl Pts',(0.294798784276878,9.43915924093234,-3.44009497706739));
#30183=CARTESIAN_POINT('Ctrl Pts',(0.354047347021712,9.93832899371509,1.47023703241122));
#30184=CARTESIAN_POINT('Ctrl Pts',(0.413295909766548,8.03882436311626,6.02571840673295));
#30185=CARTESIAN_POINT('Ctrl Pts',(0.472544472511384,4.19910182337586,9.12685748071474));
#30186=CARTESIAN_POINT('Ctrl Pts',(0.531793035256219,-0.654098512982282,
10.0251746688745));
#30187=CARTESIAN_POINT('Ctrl Pts',(0.591041598001053,-5.34942879018335,
8.50385839223102));
#30188=CARTESIAN_POINT('Ctrl Pts',(0.650290160745887,-8.75364187343509,
4.9300823360043));
#30189=CARTESIAN_POINT('Ctrl Pts',(0.709538723490721,-10.0451135486074,
0.166408114964229));
#30190=CARTESIAN_POINT('Ctrl Pts',(0.768787286235557,-8.91213420796575,
-4.637441950575));
#30191=CARTESIAN_POINT('Ctrl Pts',(0.828035848980392,-5.62816531801462,
-8.32199430859616));
#30192=CARTESIAN_POINT('Ctrl Pts',(0.887284411725228,-0.985792475144742,
-9.99802987535393));
#30193=CARTESIAN_POINT('Ctrl Pts',(0.946532974470062,3.89448213486398,-9.26089351818321));
#30194=CARTESIAN_POINT('Ctrl Pts',(1.0057815372149,7.83484888772788,-6.28875637178055));
#30195=CARTESIAN_POINT('Ctrl Pts',(1.06503009995973,9.88413496211296,-1.79846062562306));
#30196=CARTESIAN_POINT('Ctrl Pts',(1.12427866270457,9.54800801276635,3.12526083781895));
#30197=CARTESIAN_POINT('Ctrl Pts',(1.1835272254494,6.90705632238448,7.29598208910701));
#30198=CARTESIAN_POINT('Ctrl Pts',(1.22302626727929,4.03555160320576,8.90048051538159));
#30199=CARTESIAN_POINT('Ctrl Pts',(1.24277578819424,2.49464822519328,9.31322804590546));
#30200=CARTESIAN_POINT('Ctrl Pts',(-8.08092526273141,7.32294389040362,-6.48509627723018));
#30201=CARTESIAN_POINT('Ctrl Pts',(-8.06117574181647,8.39592381863735,-5.27349178069048));
#30202=CARTESIAN_POINT('Ctrl Pts',(-8.02167669998657,9.92797148557023,-2.30875446498139));
#30203=CARTESIAN_POINT('Ctrl Pts',(-7.96242813724176,9.82880183853739,2.69858166596329));
#30204=CARTESIAN_POINT('Ctrl Pts',(-7.9031795744969,7.35781851876972,7.05329954423695));
#30205=CARTESIAN_POINT('Ctrl Pts',(-7.84393101175208,3.11077563954764,9.70630784040932));
#30206=CARTESIAN_POINT('Ctrl Pts',(-7.78468244900724,-1.88696580672517,
10.0163096700013));
#30207=CARTESIAN_POINT('Ctrl Pts',(-7.7254338862624,-6.42933139469688,7.90898742424441));
#30208=CARTESIAN_POINT('Ctrl Pts',(-7.66618532351757,-9.41991164186956,
3.89269554661848));
#30209=CARTESIAN_POINT('Ctrl Pts',(-7.60693676077273,-10.1369551341012,
-1.06307544883298));
#30210=CARTESIAN_POINT('Ctrl Pts',(-7.5476881980279,-8.40737702072891,-5.76229070180903));
#30211=CARTESIAN_POINT('Ctrl Pts',(-7.48843963528306,-4.64863268122753,
-9.07073070640136));
#30212=CARTESIAN_POINT('Ctrl Pts',(-7.42919107253823,0.23208866289055,-10.1899026181865));
#30213=CARTESIAN_POINT('Ctrl Pts',(-7.36994250979339,5.05679298620976,-8.84967799296175));
#30214=CARTESIAN_POINT('Ctrl Pts',(-7.31069394704856,8.66101097414312,-5.37353298305073));
#30215=CARTESIAN_POINT('Ctrl Pts',(-7.25144538430373,10.1748424845305,-0.600453137120963));
#30216=CARTESIAN_POINT('Ctrl Pts',(-7.19219682155888,9.23291576111782,4.31754916391827));
#30217=CARTESIAN_POINT('Ctrl Pts',(-7.13294825881406,6.06257016523153,8.19348568982741));
#30218=CARTESIAN_POINT('Ctrl Pts',(-7.07369969606921,1.42898746173764,10.0918758877297));
#30219=CARTESIAN_POINT('Ctrl Pts',(-7.01445113332439,-3.54948983298891,
9.55453224832087));
#30220=CARTESIAN_POINT('Ctrl Pts',(-6.95520257057954,-7.67127676413759,
6.71114573860529));
#30221=CARTESIAN_POINT('Ctrl Pts',(-6.89595400783472,-9.94155570690313,
2.24798455074812));
#30222=CARTESIAN_POINT('Ctrl Pts',(-6.83670544508988,-9.81238141003462,
-2.7577410056674));
#30223=CARTESIAN_POINT('Ctrl Pts',(-6.77745688234504,-7.31493085792997,
-7.09786946410221));
#30224=CARTESIAN_POINT('Ctrl Pts',(-6.71820831960022,-3.05197850216906,
-9.72488517251122));
#30225=CARTESIAN_POINT('Ctrl Pts',(-6.65895975685537,1.94758690568939,-10.0047423571369));
#30226=CARTESIAN_POINT('Ctrl Pts',(-6.59971119411055,6.47709070140057,-7.8698958340312));
#30227=CARTESIAN_POINT('Ctrl Pts',(-6.5404626313657,9.44331036856071,-3.83560343017826));
#30228=CARTESIAN_POINT('Ctrl Pts',(-6.48121406862087,10.1303312566116,1.12443453456516));
#30229=CARTESIAN_POINT('Ctrl Pts',(-6.42196550587604,8.37233681299167,5.8130835776728));
#30230=CARTESIAN_POINT('Ctrl Pts',(-6.3627169431312,4.59362938864533,9.09871053670815));
#30231=CARTESIAN_POINT('Ctrl Pts',(-6.30346838038637,-0.293777642722069,
10.188309923035));
#30232=CARTESIAN_POINT('Ctrl Pts',(-6.24421981764153,-5.11027970342329,
8.8189004838395));
#30233=CARTESIAN_POINT('Ctrl Pts',(-6.1849712548967,-8.69338554959525,5.32099728220349));
#30234=CARTESIAN_POINT('Ctrl Pts',(-6.12572269215187,-10.1782914046486,
0.538839932791344));
#30235=CARTESIAN_POINT('Ctrl Pts',(-6.06647412940702,-9.20660646282684,
-4.37336961961261));
#30236=CARTESIAN_POINT('Ctrl Pts',(-6.0072255666622,-6.01285262870474,-8.23004056226918));
#30237=CARTESIAN_POINT('Ctrl Pts',(-5.94797700391735,-1.36786126920608,
-10.1003425654441));
#30238=CARTESIAN_POINT('Ctrl Pts',(-5.88872844117253,3.60727149337718,-9.53286718486024));
#30239=CARTESIAN_POINT('Ctrl Pts',(-5.82947987842769,7.711767957572,-6.6645779581067));
#30240=CARTESIAN_POINT('Ctrl Pts',(-5.77023131568285,9.95498363906506,-2.18775344521796));
#30241=CARTESIAN_POINT('Ctrl Pts',(-5.71098275293802,9.79550517293285,2.8170982940185));
#30242=CARTESIAN_POINT('Ctrl Pts',(-5.65173419019318,7.27182362969249,7.14202670743828));
#30243=CARTESIAN_POINT('Ctrl Pts',(-5.59248562744835,2.99304446790236,9.74318475675563));
#30244=CARTESIAN_POINT('Ctrl Pts',(-5.53323706470351,-2.0081236688321,9.99276757068793));
#30245=CARTESIAN_POINT('Ctrl Pts',(-5.47398850195868,-6.524619287585,7.83053686174773));
#30246=CARTESIAN_POINT('Ctrl Pts',(-5.41473993921384,-9.46635947266288,
3.77835979301097));
#30247=CARTESIAN_POINT('Ctrl Pts',(-5.35549137646901,-10.1233378410533,
-1.18574674657548));
#30248=CARTESIAN_POINT('Ctrl Pts',(-5.29624281372418,-8.33698877998584,
-5.86366629963766));
#30249=CARTESIAN_POINT('Ctrl Pts',(-5.23699425097934,-4.5384581948942,-9.12635532972027));
#30250=CARTESIAN_POINT('Ctrl Pts',(-5.17774568823451,0.355456103468731,
-10.1863445528621));
#30251=CARTESIAN_POINT('Ctrl Pts',(-5.11849712548966,5.16357897007176,-8.78779930420289));
#30252=CARTESIAN_POINT('Ctrl Pts',(-5.05924856274484,8.72544152907295,-5.26826674664877));
#30253=CARTESIAN_POINT('Ctrl Pts',(-5.,10.1813671968188,-0.477206867780972));
#30254=CARTESIAN_POINT('Ctrl Pts',(-4.94075143725517,9.17995970706714,4.429029709512));
#30255=CARTESIAN_POINT('Ctrl Pts',(-4.88150287451032,5.96291467703338,8.26629378533911));
#30256=CARTESIAN_POINT('Ctrl Pts',(-4.82225431176551,1.30668494145425,10.1084389919954));
#30257=CARTESIAN_POINT('Ctrl Pts',(-4.76300574902065,-3.66492092887833,
9.51085269448463));
#30258=CARTESIAN_POINT('Ctrl Pts',(-4.70375718627583,-7.75197646878442,
6.61776587818947));
#30259=CARTESIAN_POINT('Ctrl Pts',(-4.64450862353099,-9.9680466641253,2.12744214796467));
#30260=CARTESIAN_POINT('Ctrl Pts',(-4.58526006078616,-9.77826987352389,
-2.87635232050094));
#30261=CARTESIAN_POINT('Ctrl Pts',(-4.52601149804132,-7.22844984720876,
-7.18592215359337));
#30262=CARTESIAN_POINT('Ctrl Pts',(-4.46676293529649,-2.93400072113927,
-9.76112719717709));
#30263=CARTESIAN_POINT('Ctrl Pts',(-4.40751437255165,2.06858682257122,-9.98042649131794));
#30264=CARTESIAN_POINT('Ctrl Pts',(-4.34826580980682,6.5719087087328,-7.79089085504336));
#30265=CARTESIAN_POINT('Ctrl Pts',(-4.28901724706198,9.48906157988604,-3.72097765704751));
#30266=CARTESIAN_POINT('Ctrl Pts',(-4.22976868431715,10.1159733465758,1.24701549408342));
#30267=CARTESIAN_POINT('Ctrl Pts',(-4.17052012157231,8.30133514808314,5.91403408430452));
#30268=CARTESIAN_POINT('Ctrl Pts',(-4.11127155882748,4.48312064038335,9.15366558898046));
#30269=CARTESIAN_POINT('Ctrl Pts',(-4.05202299608264,-0.417121534692773,
10.1840057942055));
#30270=CARTESIAN_POINT('Ctrl Pts',(-3.99277443333782,-5.21668896166365,
8.75637600085633));
#30271=CARTESIAN_POINT('Ctrl Pts',(-3.93352587059297,-8.75717767061589,
5.2153430986257));
#30272=CARTESIAN_POINT('Ctrl Pts',(-3.87427730784814,-10.1840697829513,
0.415556310376332));
#30273=CARTESIAN_POINT('Ctrl Pts',(-3.8150287451033,-9.15297645265046,-4.48452744983706));
#30274=CARTESIAN_POINT('Ctrl Pts',(-3.75578018235847,-5.91275815002565,
-8.30224400089647));
#30275=CARTESIAN_POINT('Ctrl Pts',(-3.69653161961363,-1.24546071613625,
-10.1161648857498));
#30276=CARTESIAN_POINT('Ctrl Pts',(-3.6372830568688,3.72243602381481,-9.48848957630887));
#30277=CARTESIAN_POINT('Ctrl Pts',(-3.57803449412397,7.79190082519069,-6.57071121884904));
#30278=CARTESIAN_POINT('Ctrl Pts',(-3.51878593137913,9.9807443025801,-2.06705286764298));
#30279=CARTESIAN_POINT('Ctrl Pts',(-3.4595373686343,9.76067614392728,2.93550091202248));
#30280=CARTESIAN_POINT('Ctrl Pts',(-3.40028880588946,7.18481110019973,7.22955419410927));
#30281=CARTESIAN_POINT('Ctrl Pts',(-3.34104024314463,2.8748494262677,9.77871183578925));
#30282=CARTESIAN_POINT('Ctrl Pts',(-3.28179168039979,-2.12897415063036,
9.96771957155015));
#30283=CARTESIAN_POINT('Ctrl Pts',(-3.22254311765496,-6.61895723138814,
7.7509592670953));
#30284=CARTESIAN_POINT('Ctrl Pts',(-3.16329455491012,-9.51141585807944,
3.66345912571588));
#30285=CARTESIAN_POINT('Ctrl Pts',(-3.10404599216529,-10.1082380431237,
-1.30823853125571));
#30286=CARTESIAN_POINT('Ctrl Pts',(-3.04479742942045,-8.26537722419904,
-5.96418508539163));
#30287=CARTESIAN_POINT('Ctrl Pts',(-2.98554886667561,-4.42761875355267,
-9.18064031341523));
#30288=CARTESIAN_POINT('Ctrl Pts',(-2.92630030393078,0.478771675998264,
-10.1812937327914));
#30289=CARTESIAN_POINT('Ctrl Pts',(-2.86705174118595,5.26960773141081,-8.72463172564731));
#30290=CARTESIAN_POINT('Ctrl Pts',(-2.80780317844111,8.78859281091049,-5.16222827809161));
#30291=CARTESIAN_POINT('Ctrl Pts',(-2.74855461569627,10.1863990639807,-0.353890520427748));
#30292=CARTESIAN_POINT('Ctrl Pts',(-2.68930605295144,9.12565768866926,4.53986080627456));
#30293=CARTESIAN_POINT('Ctrl Pts',(-2.63005749020661,5.86238488620854,8.33788989115769));
#30294=CARTESIAN_POINT('Ctrl Pts',(-2.57080892746177,1.18419083747417,10.1235199635087));
#30295=CARTESIAN_POINT('Ctrl Pts',(-2.51156036471694,-3.77981466992552,
9.46577865007057));
#30296=CARTESIAN_POINT('Ctrl Pts',(-2.4523118019721,-7.83153956333209,6.52341570491109));
#30297=CARTESIAN_POINT('Ctrl Pts',(-2.39306323922726,-9.99307608898748,
2.00658781786958));
#30298=CARTESIAN_POINT('Ctrl Pts',(-2.33381467648243,-9.74272462905507,
-2.99454190044487));
#30299=CARTESIAN_POINT('Ctrl Pts',(-2.2745661137376,-7.14090898827806,-7.2729212296192));
#30300=CARTESIAN_POINT('Ctrl Pts',(-2.21531755099276,-2.81559275152503,
-9.79593802801323));
#30301=CARTESIAN_POINT('Ctrl Pts',(-2.15606898824792,2.18928343946426,-9.95464727716678));
#30302=CARTESIAN_POINT('Ctrl Pts',(-2.0968204255031,6.66576313095033,-7.71074356162747));
#30303=CARTESIAN_POINT('Ctrl Pts',(-2.03757186275825,9.53342148782944,-3.60580630740307));
#30304=CARTESIAN_POINT('Ctrl Pts',(-1.97832330001343,10.1001322142407,1.36941361391379));
#30305=CARTESIAN_POINT('Ctrl Pts',(-1.91907473726858,8.2291163263995,6.0141174645746));
#30306=CARTESIAN_POINT('Ctrl Pts',(-1.85982617452376,4.37195456886755,9.20727851424482));
#30307=CARTESIAN_POINT('Ctrl Pts',(-1.80057761177892,-0.540404267550662,
10.1782084680325));
#30308=CARTESIAN_POINT('Ctrl Pts',(-1.74132904903408,-5.32233333953408,
8.69256764218722));
#30309=CARTESIAN_POINT('Ctrl Pts',(-1.68208048628925,-8.81968579841007,
5.10892423201202));
#30310=CARTESIAN_POINT('Ctrl Pts',(-1.62283192354441,-10.1883549545254,
0.292211758343243));
#30311=CARTESIAN_POINT('Ctrl Pts',(-1.56358336079958,-9.09800441651432,
-4.59502775053671));
#30312=CARTESIAN_POINT('Ctrl Pts',(-1.50433479805474,-5.81179673205382,
-8.37323014949454));
#30313=CARTESIAN_POINT('Ctrl Pts',(-1.44508623530991,-1.12287755136383,
-10.1305039556658));
#30314=CARTESIAN_POINT('Ctrl Pts',(-1.38583767256507,3.83705476395099,-9.44272074825668));
#30315=CARTESIAN_POINT('Ctrl Pts',(-1.32658910982024,7.87089123021942,-6.47588107002986));
#30316=CARTESIAN_POINT('Ctrl Pts',(-1.2673405470754,10.0050415713161,-1.94604921503846));
#30317=CARTESIAN_POINT('Ctrl Pts',(-1.20809198433057,9.72441598693415,3.05347312157412));
#30318=CARTESIAN_POINT('Ctrl Pts',(-1.14884342158573,7.09674512071032,7.31602167047027));
#30319=CARTESIAN_POINT('Ctrl Pts',(-1.0895948588409,2.75623286901131,9.81280514240945));
#30320=CARTESIAN_POINT('Ctrl Pts',(-1.03034629609607,-2.24951247838848,
9.94121008734307));
#30321=CARTESIAN_POINT('Ctrl Pts',(-0.97109773335123,-6.71232469171219,
7.67024521277815));
#30322=CARTESIAN_POINT('Ctrl Pts',(-0.911849170606395,-9.55507766250236,
3.54802131541876));
#30323=CARTESIAN_POINT('Ctrl Pts',(-0.85260060786156,-10.0916561570523,
-1.43053849963697));
#30324=CARTESIAN_POINT('Ctrl Pts',(-0.793352045116725,-8.19255378385643,
-6.06382939154229));
#30325=CARTESIAN_POINT('Ctrl Pts',(-0.734103482371892,-4.31613012674232,
-9.23357921502578));
#30326=CARTESIAN_POINT('Ctrl Pts',(-0.674854919627057,0.602017050158339,
-10.1747501130201));
#30327=CARTESIAN_POINT('Ctrl Pts',(-0.615606356882222,5.37486385333546,
-8.66018492581331));
#30328=CARTESIAN_POINT('Ctrl Pts',(-0.556357794137386,8.85045549337507,
-5.05543291428316));
#30329=CARTESIAN_POINT('Ctrl Pts',(-0.497109231392552,10.1899373828937,
-0.230522285017434));
#30330=CARTESIAN_POINT('Ctrl Pts',(-0.437860668647717,9.07001764983207,
4.65002626045691));
#30331=CARTESIAN_POINT('Ctrl Pts',(-0.378612105902882,5.76099554192171,
8.40826348044112));
#30332=CARTESIAN_POINT('Ctrl Pts',(-0.319363543158047,1.06152310526953,
10.1371166062964));
#30333=CARTESIAN_POINT('Ctrl Pts',(-0.260114980413212,-3.89415420766704,
9.41931671592008));
#30334=CARTESIAN_POINT('Ctrl Pts',(-0.200866417668378,-7.90995438347004,
6.42810905691977));
#30335=CARTESIAN_POINT('Ctrl Pts',(-0.141617854923542,-10.0166403108002,
1.88543927767054));
#30336=CARTESIAN_POINT('Ctrl Pts',(-0.0823692921787074,-9.7057508889944,
-3.11229241414054));
#30337=CARTESIAN_POINT('Ctrl Pts',(-0.0231207294338736,-7.05232111575499,
-7.35885393890494));
#30338=CARTESIAN_POINT('Ctrl Pts',(0.0361278333109621,-2.69677195577391,
-9.82931255660071));
#30339=CARTESIAN_POINT('Ctrl Pts',(0.0953763960557961,2.3096590619082,-9.9274085025469));
#30340=CARTESIAN_POINT('Ctrl Pts',(0.154624958800632,6.75864020258194,-7.62946568975753));
#30341=CARTESIAN_POINT('Ctrl Pts',(0.213873521545465,9.57638359665701,-3.49010629744142));
#30342=CARTESIAN_POINT('Ctrl Pts',(0.273122084290301,10.0828101660666,1.49161100485786));
#30343=CARTESIAN_POINT('Ctrl Pts',(0.332370647035135,8.15569096806016,6.11331893396601));
#30344=CARTESIAN_POINT('Ctrl Pts',(0.391619209779972,4.26014741309707,9.25954166429657));
#30345=CARTESIAN_POINT('Ctrl Pts',(0.450867772524807,-0.663607648778533,
10.1709183839501));
#30346=CARTESIAN_POINT('Ctrl Pts',(0.510116335269641,-5.42719757239065,
8.62748555639489));
#30347=CARTESIAN_POINT('Ctrl Pts',(0.569364898014475,-8.8809003331841,5.00175475459157));
#30348=CARTESIAN_POINT('Ctrl Pts',(0.628613460759309,-10.1911471305933,
0.168827318389068));
#30349=CARTESIAN_POINT('Ctrl Pts',(0.687862023504144,-9.04169679331941,
-4.7048600296258));
#30350=CARTESIAN_POINT('Ctrl Pts',(0.747110586248981,-5.70998630863076,
-8.44297757396894));
#30351=CARTESIAN_POINT('Ctrl Pts',(0.806359148993815,-1.0001237025165,-10.1433789655793));
#30352=CARTESIAN_POINT('Ctrl Pts',(0.865607711738651,3.95109923265809,-9.39552628727104));
#30353=CARTESIAN_POINT('Ctrl Pts',(0.924856274483485,7.94875014348341,-6.38018088527799));
#30354=CARTESIAN_POINT('Ctrl Pts',(0.984104837228319,10.0278282739272,-1.82460623820867));
#30355=CARTESIAN_POINT('Ctrl Pts',(1.04335339997315,9.68681478724308,3.17069517089827));
#30356=CARTESIAN_POINT('Ctrl Pts',(1.10260196271799,7.0074695402994,7.40204942158881));
#30357=CARTESIAN_POINT('Ctrl Pts',(1.14210100454788,4.09421953692831,9.02987368199615));
#30358=CARTESIAN_POINT('Ctrl Pts',(1.16185052546282,2.53091485516785,9.44862164248496));
#30359=CARTESIAN_POINT('Ctrl Pts',(-8.16185052546282,7.42787768375328,-6.57802417109255));
#30360=CARTESIAN_POINT('Ctrl Pts',(-8.14210100454788,8.51623282935078,-5.34905804270585));
#30361=CARTESIAN_POINT('Ctrl Pts',(-8.102601962718,10.070233904051,-2.34183765769039));
#30362=CARTESIAN_POINT('Ctrl Pts',(-8.04335339997314,9.96964321004528,2.73725086992161));
#30363=CARTESIAN_POINT('Ctrl Pts',(-7.98410483722833,7.4632520465296,7.15436948112095));
#30364=CARTESIAN_POINT('Ctrl Pts',(-7.92485627448348,3.15535135841191,9.84539393970996));
#30365=CARTESIAN_POINT('Ctrl Pts',(-7.86560771173865,-1.91400499792807,
10.1598379265015));
#30366=CARTESIAN_POINT('Ctrl Pts',(-7.80635914899382,-6.52146020819656,
8.0223189019126));
#30367=CARTESIAN_POINT('Ctrl Pts',(-7.74711058624898,-9.55489383979345,
3.94847575143437));
#30368=CARTESIAN_POINT('Ctrl Pts',(-7.68786202350415,-10.2822121743239,
-1.07830874040703));
#30369=CARTESIAN_POINT('Ctrl Pts',(-7.62861346075931,-8.5278501495838,-5.84486118586212));
#30370=CARTESIAN_POINT('Ctrl Pts',(-7.56936489801448,-4.71524505303195,
-9.20070933189968));
#30371=CARTESIAN_POINT('Ctrl Pts',(-7.51011633526964,0.23541436689089,-10.3359183669881));
#30372=CARTESIAN_POINT('Ctrl Pts',(-7.4508677725248,5.12925407264827,-8.97648905359836));
#30373=CARTESIAN_POINT('Ctrl Pts',(-7.39161920977998,8.78511853926469,-5.45053278095167));
#30374=CARTESIAN_POINT('Ctrl Pts',(-7.33237064703513,10.3206424298279,-0.609057303198129));
#30375=CARTESIAN_POINT('Ctrl Pts',(-7.27312208429031,9.36521841002403,4.37941728943228));
#30376=CARTESIAN_POINT('Ctrl Pts',(-7.21387352154547,6.14944349027773,8.31089387252787));
#30377=CARTESIAN_POINT('Ctrl Pts',(-7.15462495880063,1.44946407295485,10.2364869669299));
#30378=CARTESIAN_POINT('Ctrl Pts',(-7.0953763960558,-3.60035208705037,9.69144348613765));
#30379=CARTESIAN_POINT('Ctrl Pts',(-7.03612783331096,-7.78120197765055,
6.80731279800296));
#30380=CARTESIAN_POINT('Ctrl Pts',(-6.97687927056613,-10.0840127798693,
2.280196943719));
#30381=CARTESIAN_POINT('Ctrl Pts',(-6.91763070782129,-9.95298748575479,
-2.79725793070895));
#30382=CARTESIAN_POINT('Ctrl Pts',(-6.85838214507646,-7.41974982889312,
-7.19957806363757));
#30383=CARTESIAN_POINT('Ctrl Pts',(-6.79913358233162,-3.09571169011194,
-9.86423747485219));
#30384=CARTESIAN_POINT('Ctrl Pts',(-6.73988501958679,1.97549476418875,-10.1481048603504));
#30385=CARTESIAN_POINT('Ctrl Pts',(-6.68063645684196,6.56990387972609,-7.98266715052507));
#30386=CARTESIAN_POINT('Ctrl Pts',(-6.62138789409711,9.57862785748067,-3.8905655360932));
#30387=CARTESIAN_POINT('Ctrl Pts',(-6.56213933135229,10.2754933802813,1.14054706838368));
#30388=CARTESIAN_POINT('Ctrl Pts',(-6.50289076860745,8.49230783477424,5.89638189594384));
#30389=CARTESIAN_POINT('Ctrl Pts',(-6.44364220586261,4.65945359325582,9.22909009791965));
#30390=CARTESIAN_POINT('Ctrl Pts',(-6.38439364311778,-0.297987316169458,
10.3343028493835));
#30391=CARTESIAN_POINT('Ctrl Pts',(-6.32514508037294,-5.18350722535756,
8.94527051955084));
#30392=CARTESIAN_POINT('Ctrl Pts',(-6.26589651762811,-8.81795702473186,
5.3972442721547));
#30393=CARTESIAN_POINT('Ctrl Pts',(-6.20664795488328,-10.3241407710909,
0.546561215243084));
#30394=CARTESIAN_POINT('Ctrl Pts',(-6.14739939213844,-9.33853211383284,
-4.43603762182241));
#30395=CARTESIAN_POINT('Ctrl Pts',(-6.08815082939361,-6.09901352855942,
-8.34797255636136));
#30396=CARTESIAN_POINT('Ctrl Pts',(-6.02890226664877,-1.38746197541141,
-10.2450749675197));
#30397=CARTESIAN_POINT('Ctrl Pts',(-5.96965370390394,3.65896172712842,-9.6694679741298));
#30398=CARTESIAN_POINT('Ctrl Pts',(-5.9104051411591,7.82227338781035,-6.76007772659941));
#30399=CARTESIAN_POINT('Ctrl Pts',(-5.85115657841427,10.097633126978,-2.21910275928568));
#30400=CARTESIAN_POINT('Ctrl Pts',(-5.79190801566943,9.93586942137656,2.85746577663947));
#30401=CARTESIAN_POINT('Ctrl Pts',(-5.7326594529246,7.37602489757785,7.24436805619533));
#30402=CARTESIAN_POINT('Ctrl Pts',(-5.67341089017976,3.03593316326608,9.88279928216156));
#30403=CARTESIAN_POINT('Ctrl Pts',(-5.61416232743494,-2.03689898614156,
10.1359584817405));
#30404=CARTESIAN_POINT('Ctrl Pts',(-5.55491376469008,-6.61811352463711,
7.94274418562801));
#30405=CARTESIAN_POINT('Ctrl Pts',(-5.49566520194526,-9.60200724267784,
3.83250162881555));
#30406=CARTESIAN_POINT('Ctrl Pts',(-5.43641663920042,-10.268399752891,-1.2027378509636));
#30407=CARTESIAN_POINT('Ctrl Pts',(-5.37716807645559,-8.45645328372782,
-5.94768944073586));
#30408=CARTESIAN_POINT('Ctrl Pts',(-5.31791951371075,-4.60349182637855,
-9.2571310257432));
#30409=CARTESIAN_POINT('Ctrl Pts',(-5.25867095096592,0.360549595630422,
-10.3323093165276));
#30410=CARTESIAN_POINT('Ctrl Pts',(-5.19942238822108,5.23757024143739,-8.91372367696696));
#30411=CARTESIAN_POINT('Ctrl Pts',(-5.14017382547626,8.85047234891796,-5.3437581367751));
#30412=CARTESIAN_POINT('Ctrl Pts',(-5.0809252627314,10.327260637686,-0.484044982014571));
#30413=CARTESIAN_POINT('Ctrl Pts',(-5.02167669998659,9.31150352459139,4.49249529046319));
#30414=CARTESIAN_POINT('Ctrl Pts',(-4.96242813724174,6.04835999326767,8.38474526835198));
#30415=CARTESIAN_POINT('Ctrl Pts',(-4.90317957449691,1.32540902423731,10.2532874114492));
#30416=CARTESIAN_POINT('Ctrl Pts',(-4.84393101175207,-3.7174372476088,9.64713802810981));
#30417=CARTESIAN_POINT('Ctrl Pts',(-4.78468244900724,-7.86305806506605,
6.71259485509974));
#30418=CARTESIAN_POINT('Ctrl Pts',(-4.7254338862624,-10.1108833380651,2.15792723402554));
#30419=CARTESIAN_POINT('Ctrl Pts',(-4.66618532351757,-9.91838714952408,
-2.91756888101505));
#30420=CARTESIAN_POINT('Ctrl Pts',(-4.60693676077273,-7.33202959243926,
-7.28889250016123));
#30421=CARTESIAN_POINT('Ctrl Pts',(-4.5476881980279,-2.97604335180359,-9.90099882797171));
#30422=CARTESIAN_POINT('Ctrl Pts',(-4.48843963528306,2.09822854390817,-10.1234405614317));
#30423=CARTESIAN_POINT('Ctrl Pts',(-4.42919107253823,6.66608057740692,-7.90253007326325));
#30424=CARTESIAN_POINT('Ctrl Pts',(-4.36994250979339,9.62503465871992,-3.77429723812952));
#30425=CARTESIAN_POINT('Ctrl Pts',(-4.31069394704856,10.2609297292228,1.26488454621852));
#30426=CARTESIAN_POINT('Ctrl Pts',(-4.25144538430372,8.42028875471895,5.99877896829557));
#30427=CARTESIAN_POINT('Ctrl Pts',(-4.19219682155889,4.54736131488258,9.28483262612855));
#30428=CARTESIAN_POINT('Ctrl Pts',(-4.13294825881405,-0.423098658862809,
10.3299370447346));
#30429=CARTESIAN_POINT('Ctrl Pts',(-4.07369969606922,-5.29144127025228,
8.88185009481599));
#30430=CARTESIAN_POINT('Ctrl Pts',(-4.01445113332439,-8.88266325206611,
5.29007612173078));
#30431=CARTESIAN_POINT('Ctrl Pts',(-3.95520257057955,-10.3300019504043,
0.421511005735301));
#30432=CARTESIAN_POINT('Ctrl Pts',(-3.89595400783472,-9.28413361485067,
-4.54878828314875));
#30433=CARTESIAN_POINT('Ctrl Pts',(-3.83670544508988,-5.99748475057414,
-8.42121063089757));
#30434=CARTESIAN_POINT('Ctrl Pts',(-3.77745688234504,-1.26330748915105,
-10.2611240130488));
#30435=CARTESIAN_POINT('Ctrl Pts',(-3.71820831960021,3.77577650249745,-9.62445445864334));
#30436=CARTESIAN_POINT('Ctrl Pts',(-3.65895975685538,7.90355451573215,-6.66486592814603));
#30437=CARTESIAN_POINT('Ctrl Pts',(-3.59971119411054,10.123762926756,-2.09667260824215));
#30438=CARTESIAN_POINT('Ctrl Pts',(-3.5404626313657,9.90054131137476,2.97756503960422));
#30439=CARTESIAN_POINT('Ctrl Pts',(-3.48121406862087,7.28776552597823,7.33314976402877));
#30440=CARTESIAN_POINT('Ctrl Pts',(-3.42196550587603,2.91604445112685,9.91883544486771));
#30441=CARTESIAN_POINT('Ctrl Pts',(-3.3627169431312,-2.15948118945414,10.1105515584317));
#30442=CARTESIAN_POINT('Ctrl Pts',(-3.30346838038637,-6.71380327974022,
7.86202628743132));
#30443=CARTESIAN_POINT('Ctrl Pts',(-3.24421981764153,-9.64770926153188,
3.71595449760403));
#30444=CARTESIAN_POINT('Ctrl Pts',(-3.1849712548967,-10.2530835830897,-1.32698487613358));
#30445=CARTESIAN_POINT('Ctrl Pts',(-3.12572269215186,-8.38381557339049,
-6.04964860588505));
#30446=CARTESIAN_POINT('Ctrl Pts',(-3.06647412940703,-4.49106411627424,
-9.31219388365737));
#30447=CARTESIAN_POINT('Ctrl Pts',(-3.00722556666219,0.485632213080447,
-10.3271861209591));
#30448=CARTESIAN_POINT('Ctrl Pts',(-2.94797700391736,5.34511833711766,-8.84965094145075));
#30449=CARTESIAN_POINT('Ctrl Pts',(-2.88872844117252,8.91452855419303,-5.23620019477759));
#30450=CARTESIAN_POINT('Ctrl Pts',(-2.82947987842769,10.3323646087608,-0.358961578638042));
#30451=CARTESIAN_POINT('Ctrl Pts',(-2.77023131568285,9.2564233878763,4.60491453641526));
#30452=CARTESIAN_POINT('Ctrl Pts',(-2.71098275293802,5.94638966535093,8.45736730733147));
#30453=CARTESIAN_POINT('Ctrl Pts',(-2.65173419019318,1.20115964653319,10.2685844850618));
#30454=CARTESIAN_POINT('Ctrl Pts',(-2.59248562744835,-3.83397735332308,
9.60141809721447));
#30455=CARTESIAN_POINT('Ctrl Pts',(-2.53323706470351,-7.94376125537936,
6.61689269527968));
#30456=CARTESIAN_POINT('Ctrl Pts',(-2.47398850195868,-10.1362714209391,
2.03534112727213));
#30457=CARTESIAN_POINT('Ctrl Pts',(-2.41473993921384,-9.88233256108192,
-3.0374520532005));
#30458=CARTESIAN_POINT('Ctrl Pts',(-2.35549137646901,-7.24323432072894,
-7.37713822551306));
#30459=CARTESIAN_POINT('Ctrl Pts',(-2.29624281372417,-2.85593866054291,
-9.93630847903426));
#30460=CARTESIAN_POINT('Ctrl Pts',(-2.23699425097934,2.22065467751534,-10.097291945197));
#30461=CARTESIAN_POINT('Ctrl Pts',(-2.1777456882345,6.76127988232371,-7.82123431283046));
#30462=CARTESIAN_POINT('Ctrl Pts',(-2.11849712548967,9.67003021995834,-3.65747554583815));
#30463=CARTESIAN_POINT('Ctrl Pts',(-2.05924856274484,10.2448616020983,1.38903656437241));
#30464=CARTESIAN_POINT('Ctrl Pts',(-2.,8.34703507669558,6.10029648883767));
#30465=CARTESIAN_POINT('Ctrl Pts',(-1.94075143725517,4.43460229417169,9.33921379538122));
#30466=CARTESIAN_POINT('Ctrl Pts',(-1.88150287451033,-0.548147966066605,
10.3240566460384));
#30467=CARTESIAN_POINT('Ctrl Pts',(-1.8222543117655,-5.39859947445838,8.8171273971566));
#30468=CARTESIAN_POINT('Ctrl Pts',(-1.76300574902066,-8.94606708725103,
5.18213233078001));
#30469=CARTESIAN_POINT('Ctrl Pts',(-1.70375718627582,-10.3343485261506,
0.296398993521226));
#30470=CARTESIAN_POINT('Ctrl Pts',(-1.64450862353099,-9.22837385940843,
-4.66087199291068));
#30471=CARTESIAN_POINT('Ctrl Pts',(-1.58526006078615,-5.89507661052875,
-8.49321397230215));
#30472=CARTESIAN_POINT('Ctrl Pts',(-1.52601149804132,-1.13896777446197,
-10.2756685540187));
#30473=CARTESIAN_POINT('Ctrl Pts',(-1.46676293529649,3.89203766668761,-9.57802978823917));
#30474=CARTESIAN_POINT('Ctrl Pts',(-1.40751437255165,7.98367681019796,-6.56867691499734));
#30475=CARTESIAN_POINT('Ctrl Pts',(-1.34826580980682,10.1484083621057,-1.97393503926917));
#30476=CARTESIAN_POINT('Ctrl Pts',(-1.28901724706198,9.86376156610162,3.09722772659819));
#30477=CARTESIAN_POINT('Ctrl Pts',(-1.22976868431715,7.19843760901787,7.42085627218239));
#30478=CARTESIAN_POINT('Ctrl Pts',(-1.17052012157231,2.79572818327685,9.95341728998352));
#30479=CARTESIAN_POINT('Ctrl Pts',(-1.11127155882748,-2.2817467657294,10.0836622077694));
#30480=CARTESIAN_POINT('Ctrl Pts',(-1.05202299608264,-6.80850864486509,
7.78015564472256));
#30481=CARTESIAN_POINT('Ctrl Pts',(-0.992774433337806,-9.69199671580699,
3.5988625264241));
#30482=CARTESIAN_POINT('Ctrl Pts',(-0.933525870592972,-10.2362640876317,
-1.45103733638162));
#30483=CARTESIAN_POINT('Ctrl Pts',(-0.874277307848137,-8.30994861285242,
-6.15072076061499));
#30484=CARTESIAN_POINT('Ctrl Pts',(-0.815028745103304,-4.37797791822729,
-9.36589137086476));
#30485=CARTESIAN_POINT('Ctrl Pts',(-0.755780182358469,0.610643626256656,
-10.3205487346842));
#30486=CARTESIAN_POINT('Ctrl Pts',(-0.696531619613634,5.45188272188197,
-8.78428065411268));
#30487=CARTESIAN_POINT('Ctrl Pts',(-0.637283056868798,8.97727769516869,
-5.12787451163251));
#30488=CARTESIAN_POINT('Ctrl Pts',(-0.578034494123964,10.3359536298547,
-0.233825543676864));
#30489=CARTESIAN_POINT('Ctrl Pts',(-0.518785931379129,9.19998605761851,
4.71665860149186));
#30490=CARTESIAN_POINT('Ctrl Pts',(-0.459537368634294,5.84354746703977,
8.52874931178039));
#30491=CARTESIAN_POINT('Ctrl Pts',(-0.400288805889459,1.07673415260668,
10.2823759603276));
#30492=CARTESIAN_POINT('Ctrl Pts',(-0.341040243144623,-3.94995531430047,
9.55429038887948));
#30493=CARTESIAN_POINT('Ctrl Pts',(-0.28179168039979,-8.02329971713674,
6.52022035498553));
#30494=CARTESIAN_POINT('Ctrl Pts',(-0.222543117654954,-10.1601733052027,
1.91245659454439));
#30495=CARTESIAN_POINT('Ctrl Pts',(-0.163294554910119,-9.84482900748493,
-3.15688986755775));
#30496=CARTESIAN_POINT('Ctrl Pts',(-0.104045992165286,-7.1533770322923,
-7.46430230367082));
#30497=CARTESIAN_POINT('Ctrl Pts',(-0.0447974294204499,-2.73541522757191,
-9.97016124642001));
#30498=CARTESIAN_POINT('Ctrl Pts',(0.0144511333243841,2.34275521699797,
-10.0696628537879));
#30499=CARTESIAN_POINT('Ctrl Pts',(0.0736996960692199,6.85548783175356,
-7.73879177337077));
#30500=CARTESIAN_POINT('Ctrl Pts',(0.132948258814054,9.7136079523817,-3.54011761781546));
#30501=CARTESIAN_POINT('Ctrl Pts',(0.192196821558889,10.2272913384181,1.51298497730451));
#30502=CARTESIAN_POINT('Ctrl Pts',(0.251445384303724,8.27255757300405,6.20091946119904));
#30503=CARTESIAN_POINT('Ctrl Pts',(0.31069394704856,4.32119300281829,9.39222584787842));
#30504=CARTESIAN_POINT('Ctrl Pts',(0.369942509793395,-0.673116784574792,
10.3166620990257));
#30505=CARTESIAN_POINT('Ctrl Pts',(0.429191072538228,-5.50496635459793,
8.7511127205588));
#30506=CARTESIAN_POINT('Ctrl Pts',(0.488439635283064,-9.00815879293313,
5.07342717317882));
#30507=CARTESIAN_POINT('Ctrl Pts',(0.547688198027897,-10.3371807125793,
0.171246521813919));
#30508=CARTESIAN_POINT('Ctrl Pts',(0.606936760772733,-9.17125937867306,
-4.77227810867661));
#30509=CARTESIAN_POINT('Ctrl Pts',(0.666185323517568,-5.7918072992469,-8.56396083934171));
#30510=CARTESIAN_POINT('Ctrl Pts',(0.725433886262404,-1.01445492988825,
-10.2887280558046));
#30511=CARTESIAN_POINT('Ctrl Pts',(0.784682449007238,4.0077163304522,-9.53015905635885));
#30512=CARTESIAN_POINT('Ctrl Pts',(0.843931011752074,8.06265139923896,-6.47160539877543));
#30513=CARTESIAN_POINT('Ctrl Pts',(0.903179574496907,10.1715215857415,-1.85075185079428));
#30514=CARTESIAN_POINT('Ctrl Pts',(0.962428137241743,9.8256215617198,3.21612950397759));
#30515=CARTESIAN_POINT('Ctrl Pts',(1.02167669998658,7.10788275821431,7.5081167540706));
#30516=CARTESIAN_POINT('Ctrl Pts',(1.06117574181647,4.15288747065086,9.15926684861071));
#30517=CARTESIAN_POINT('Ctrl Pts',(1.08092526273141,2.56718148514241,9.58401523906446));
#30518=CARTESIAN_POINT('Ctrl Pts',(-8.24277578819424,7.53281147710294,-6.67095206495492));
#30519=CARTESIAN_POINT('Ctrl Pts',(-8.22302626727929,8.6365418400642,-5.42462430472122));
#30520=CARTESIAN_POINT('Ctrl Pts',(-8.1835272254494,10.2124963225319,-2.3749208503994));
#30521=CARTESIAN_POINT('Ctrl Pts',(-8.12427866270457,10.1104845815532,2.77592007387994));
#30522=CARTESIAN_POINT('Ctrl Pts',(-8.06503009995973,7.56868557428947,7.25543941800496));
#30523=CARTESIAN_POINT('Ctrl Pts',(-8.0057815372149,3.19992707727617,9.98448003901059));
#30524=CARTESIAN_POINT('Ctrl Pts',(-7.94653297447006,-1.94104418913098,
10.3033661830017));
#30525=CARTESIAN_POINT('Ctrl Pts',(-7.88728441172523,-6.61358902169624,
8.13565037958078));
#30526=CARTESIAN_POINT('Ctrl Pts',(-7.82803584898039,-9.68987603771733,
4.00425595625027));
#30527=CARTESIAN_POINT('Ctrl Pts',(-7.76878728623556,-10.4274692145465,
-1.09354203198108));
#30528=CARTESIAN_POINT('Ctrl Pts',(-7.70953872349072,-8.64832327843871,
-5.92743166991522));
#30529=CARTESIAN_POINT('Ctrl Pts',(-7.65029016074589,-4.78185742483636,
-9.33068795739798));
#30530=CARTESIAN_POINT('Ctrl Pts',(-7.59104159800105,0.238740070891225,
-10.4819341157898));
#30531=CARTESIAN_POINT('Ctrl Pts',(-7.53179303525622,5.20171515908679,-9.10330011423497));
#30532=CARTESIAN_POINT('Ctrl Pts',(-7.47254447251139,8.90922610438627,-5.52753257885261));
#30533=CARTESIAN_POINT('Ctrl Pts',(-7.41329590976654,10.4664423751253,-0.617661469275298));
#30534=CARTESIAN_POINT('Ctrl Pts',(-7.35404734702172,9.49752105893024,4.4412854149463));
#30535=CARTESIAN_POINT('Ctrl Pts',(-7.29479878427687,6.23631681532395,8.42830205522834));
#30536=CARTESIAN_POINT('Ctrl Pts',(-7.23555022153205,1.46994068417205,10.38109804613));
#30537=CARTESIAN_POINT('Ctrl Pts',(-7.17630165878721,-3.65121434111183,
9.82835472395443));
#30538=CARTESIAN_POINT('Ctrl Pts',(-7.11705309604238,-7.89112719116351,
6.90347985740062));
#30539=CARTESIAN_POINT('Ctrl Pts',(-7.05780453329754,-10.2264698528354,
2.31240933668989));
#30540=CARTESIAN_POINT('Ctrl Pts',(-6.9985559705527,-10.0935935614749,-2.8367748557505));
#30541=CARTESIAN_POINT('Ctrl Pts',(-6.93930740780787,-7.52456879985629,
-7.30128666317293));
#30542=CARTESIAN_POINT('Ctrl Pts',(-6.88005884506304,-3.13944487805482,
-10.0035897771931));
#30543=CARTESIAN_POINT('Ctrl Pts',(-6.8208102823182,2.0034026226881,-10.2914673635639));
#30544=CARTESIAN_POINT('Ctrl Pts',(-6.76156171957337,6.6627170580516,-8.09543846701894));
#30545=CARTESIAN_POINT('Ctrl Pts',(-6.70231315682853,9.71394534640064,-3.94552764200815));
#30546=CARTESIAN_POINT('Ctrl Pts',(-6.6430645940837,10.4206555039509,1.1566596022022));
#30547=CARTESIAN_POINT('Ctrl Pts',(-6.58381603133886,8.61227885655681,5.97968021421488));
#30548=CARTESIAN_POINT('Ctrl Pts',(-6.52456746859403,4.72527779786631,9.35946965913116));
#30549=CARTESIAN_POINT('Ctrl Pts',(-6.46531890584919,-0.302196989616849,
10.480295775732));
#30550=CARTESIAN_POINT('Ctrl Pts',(-6.40607034310435,-5.25673474729183,
9.07164055526217));
#30551=CARTESIAN_POINT('Ctrl Pts',(-6.34682178035952,-8.94252849986846,
5.4734912621059));
#30552=CARTESIAN_POINT('Ctrl Pts',(-6.28757321761469,-10.4699901375332,
0.554282497694829));
#30553=CARTESIAN_POINT('Ctrl Pts',(-6.22832465486985,-9.47045776483884,
-4.49870562403222));
#30554=CARTESIAN_POINT('Ctrl Pts',(-6.16907609212502,-6.18517442841409,
-8.46590455045353));
#30555=CARTESIAN_POINT('Ctrl Pts',(-6.10982752938018,-1.40706268161673,
-10.3898073695953));
#30556=CARTESIAN_POINT('Ctrl Pts',(-6.05057896663535,3.71065196087965,-9.80606876339935));
#30557=CARTESIAN_POINT('Ctrl Pts',(-5.99133040389051,7.93277881804871,-6.85557749509213));
#30558=CARTESIAN_POINT('Ctrl Pts',(-5.93208184114569,10.2402826148908,-2.25045207335339));
#30559=CARTESIAN_POINT('Ctrl Pts',(-5.87283327840083,10.0762336698203,2.89783325926043));
#30560=CARTESIAN_POINT('Ctrl Pts',(-5.81358471565602,7.4802261654632,7.34670940495238));
#30561=CARTESIAN_POINT('Ctrl Pts',(-5.75433615291117,3.07882185862981,10.0224138075675));
#30562=CARTESIAN_POINT('Ctrl Pts',(-5.69508759016634,-2.06567430345103,
10.2791493927931));
#30563=CARTESIAN_POINT('Ctrl Pts',(-5.63583902742151,-6.7116077616892,8.05495150950825));
#30564=CARTESIAN_POINT('Ctrl Pts',(-5.57659046467666,-9.73765501269281,
3.88664346462016));
#30565=CARTESIAN_POINT('Ctrl Pts',(-5.51734190193184,-10.4134616647286,
-1.21972895535173));
#30566=CARTESIAN_POINT('Ctrl Pts',(-5.458093339187,-8.57591778746981,-6.03171258183405));
#30567=CARTESIAN_POINT('Ctrl Pts',(-5.39884477644216,-4.6685254578629,-9.38790672176614));
#30568=CARTESIAN_POINT('Ctrl Pts',(-5.33959621369733,0.365643087792113,
-10.4782740801931));
#30569=CARTESIAN_POINT('Ctrl Pts',(-5.2803476509525,5.31156151280302,-9.03964804973101));
#30570=CARTESIAN_POINT('Ctrl Pts',(-5.22109908820765,8.975503168763,-5.41924952690144));
#30571=CARTESIAN_POINT('Ctrl Pts',(-5.16185052546283,10.4731540785531,-0.490883096248158));
#30572=CARTESIAN_POINT('Ctrl Pts',(-5.10260196271799,9.44304734211565,4.55596087141438));
#30573=CARTESIAN_POINT('Ctrl Pts',(-5.04335339997316,6.13380530950194,8.50319675136485));
#30574=CARTESIAN_POINT('Ctrl Pts',(-4.98410483722832,1.34413310702038,10.3981358309029));
#30575=CARTESIAN_POINT('Ctrl Pts',(-4.92485627448348,-3.76995356633927,
9.78342336173498));
#30576=CARTESIAN_POINT('Ctrl Pts',(-4.86560771173865,-7.97413966134769,
6.80742383201003));
#30577=CARTESIAN_POINT('Ctrl Pts',(-4.80635914899381,-10.2537200120049,
2.1884123200864));
#30578=CARTESIAN_POINT('Ctrl Pts',(-4.74711058624898,-10.0585044255243,
-2.95878544152915));
#30579=CARTESIAN_POINT('Ctrl Pts',(-4.68786202350414,-7.43560933766978,
-7.3918628467291));
#30580=CARTESIAN_POINT('Ctrl Pts',(-4.62861346075931,-3.01808598246791,
-10.0408704587663));
#30581=CARTESIAN_POINT('Ctrl Pts',(-4.56936489801447,2.12787026524513,-10.2664546315455));
#30582=CARTESIAN_POINT('Ctrl Pts',(-4.51011633526964,6.76025244608102,-8.01416929148315));
#30583=CARTESIAN_POINT('Ctrl Pts',(-4.4508677725248,9.7610077375538,-3.82761681921153));
#30584=CARTESIAN_POINT('Ctrl Pts',(-4.39161920977998,10.4058861118699,1.28275359835361));
#30585=CARTESIAN_POINT('Ctrl Pts',(-4.33237064703513,8.53924236135476,6.08352385228661));
#30586=CARTESIAN_POINT('Ctrl Pts',(-4.2731220842903,4.61160198938182,9.41599966327665));
#30587=CARTESIAN_POINT('Ctrl Pts',(-4.21387352154547,-0.429075783032848,
10.4758682952637));
#30588=CARTESIAN_POINT('Ctrl Pts',(-4.15462495880063,-5.3661935788409,9.00732418877565));
#30589=CARTESIAN_POINT('Ctrl Pts',(-4.09537639605579,-9.00814883351634,
5.36480914483585));
#30590=CARTESIAN_POINT('Ctrl Pts',(-4.03612783331096,-10.4759341178572,
0.427465701094278));
#30591=CARTESIAN_POINT('Ctrl Pts',(-3.97687927056613,-9.41529077705088,
-4.61304911646044));
#30592=CARTESIAN_POINT('Ctrl Pts',(-3.91763070782129,-6.08221135112264,
-8.54017726089867));
#30593=CARTESIAN_POINT('Ctrl Pts',(-3.85838214507646,-1.28115426216585,
-10.4060831403478));
#30594=CARTESIAN_POINT('Ctrl Pts',(-3.79913358233163,3.8291169811801,-9.76041934097784));
#30595=CARTESIAN_POINT('Ctrl Pts',(-3.73988501958678,8.01520820627361,-6.75902063744299));
#30596=CARTESIAN_POINT('Ctrl Pts',(-3.68063645684196,10.2667815509319,-2.12629234884133));
#30597=CARTESIAN_POINT('Ctrl Pts',(-3.62138789409711,10.0404064788223,3.01962916718597));
#30598=CARTESIAN_POINT('Ctrl Pts',(-3.56213933135229,7.39071995175672,7.43674533394825));
#30599=CARTESIAN_POINT('Ctrl Pts',(-3.50289076860744,2.95723947598601,10.0589590539462));
#30600=CARTESIAN_POINT('Ctrl Pts',(-3.44364220586262,-2.18998822827795,
10.2533835453132));
#30601=CARTESIAN_POINT('Ctrl Pts',(-3.38439364311777,-6.80864932809227,
7.97309330776734));
#30602=CARTESIAN_POINT('Ctrl Pts',(-3.32514508037295,-9.78400266498433,
3.76844986949217));
#30603=CARTESIAN_POINT('Ctrl Pts',(-3.26589651762811,-10.3979291230557,
-1.34573122101146));
#30604=CARTESIAN_POINT('Ctrl Pts',(-3.20664795488328,-8.50225392258195,
-6.13511212637845));
#30605=CARTESIAN_POINT('Ctrl Pts',(-3.14739939213844,-4.55450947899581,
-9.44374745389952));
#30606=CARTESIAN_POINT('Ctrl Pts',(-3.08815082939361,0.492492750162627,
-10.4730785091268));
#30607=CARTESIAN_POINT('Ctrl Pts',(-3.02890226664877,5.42062894282451,-8.97467015725421));
#30608=CARTESIAN_POINT('Ctrl Pts',(-2.96965370390394,9.04046429747557,-5.31017211146357));
#30609=CARTESIAN_POINT('Ctrl Pts',(-2.9104051411591,10.478330153541,-0.36403263684834));
#30610=CARTESIAN_POINT('Ctrl Pts',(-2.85115657841426,9.38718908708332,4.66996826655597));
#30611=CARTESIAN_POINT('Ctrl Pts',(-2.79190801566943,6.03039444449335,8.57684472350524));
#30612=CARTESIAN_POINT('Ctrl Pts',(-2.7326594529246,1.21812845559219,10.4136490066149));
#30613=CARTESIAN_POINT('Ctrl Pts',(-2.67341089017976,-3.88814003672063,
9.73705754435836));
#30614=CARTESIAN_POINT('Ctrl Pts',(-2.61416232743493,-8.05598294742662,
6.71036968564828));
#30615=CARTESIAN_POINT('Ctrl Pts',(-2.55491376469009,-10.2794667528907,
2.06409443667468));
#30616=CARTESIAN_POINT('Ctrl Pts',(-2.49566520194525,-10.0219404931087,
-3.08036220595614));
#30617=CARTESIAN_POINT('Ctrl Pts',(-2.43641663920042,-7.34555965317983,
-7.48135522140693));
#30618=CARTESIAN_POINT('Ctrl Pts',(-2.37716807645559,-2.8962845695608,-10.0766789300553));
#30619=CARTESIAN_POINT('Ctrl Pts',(-2.31791951371075,2.25202591556642,-10.2399366132273));
#30620=CARTESIAN_POINT('Ctrl Pts',(-2.25867095096592,6.85679663369709,-7.93172506403346));
#30621=CARTESIAN_POINT('Ctrl Pts',(-2.19942238822108,9.80663895208724,-3.70914478427321));
#30622=CARTESIAN_POINT('Ctrl Pts',(-2.14017382547625,10.3895909899559,1.40865951483102));
#30623=CARTESIAN_POINT('Ctrl Pts',(-2.08092526273141,8.46495382699166,6.18647551310075));
#30624=CARTESIAN_POINT('Ctrl Pts',(-2.02167669998658,4.49725001947583,9.47114907651764));
#30625=CARTESIAN_POINT('Ctrl Pts',(-1.96242813724174,-0.555891664582547,
10.4699048240442));
#30626=CARTESIAN_POINT('Ctrl Pts',(-1.90317957449691,-5.47486560938269,
8.941687152126));
#30627=CARTESIAN_POINT('Ctrl Pts',(-1.84393101175207,-9.072448376092,5.25534042954797));
#30628=CARTESIAN_POINT('Ctrl Pts',(-1.78468244900724,-10.4803420977758,
0.300586228699219));
#30629=CARTESIAN_POINT('Ctrl Pts',(-1.7254338862624,-9.35874330230254,-4.72671623528466));
#30630=CARTESIAN_POINT('Ctrl Pts',(-1.66618532351757,-5.97835648900369,
-8.61319779510975));
#30631=CARTESIAN_POINT('Ctrl Pts',(-1.60693676077273,-1.15505799756011,
-10.4208331523717));
#30632=CARTESIAN_POINT('Ctrl Pts',(-1.5476881980279,3.94702056942422,-9.71333882822164));
#30633=CARTESIAN_POINT('Ctrl Pts',(-1.48843963528306,8.0964623901765,-6.66147275996483));
#30634=CARTESIAN_POINT('Ctrl Pts',(-1.42919107253823,10.2917751528953,-2.00182086349988));
#30635=CARTESIAN_POINT('Ctrl Pts',(-1.36994250979339,10.0031071452691,3.14098233162225));
#30636=CARTESIAN_POINT('Ctrl Pts',(-1.31069394704856,7.30013009732543,7.52569087389453));
#30637=CARTESIAN_POINT('Ctrl Pts',(-1.25144538430372,2.83522349754239,10.0940294375576));
#30638=CARTESIAN_POINT('Ctrl Pts',(-1.19219682155889,-2.31398105307032,
10.2261143281957));
#30639=CARTESIAN_POINT('Ctrl Pts',(-1.13294825881405,-6.90469259801799,
7.89006607666695));
#30640=CARTESIAN_POINT('Ctrl Pts',(-1.07369969606922,-9.82891576911162,
3.64970373742945));
#30641=CARTESIAN_POINT('Ctrl Pts',(-1.01445113332438,-10.380872018211,-1.47153617312628));
#30642=CARTESIAN_POINT('Ctrl Pts',(-0.955202570579548,-8.42734344184841,
-6.23761212968768));
#30643=CARTESIAN_POINT('Ctrl Pts',(-0.895954007834717,-4.43982570971225,
-9.49820352670374));
#30644=CARTESIAN_POINT('Ctrl Pts',(-0.836705445089881,0.619270202354978,
-10.4663473563483));
#30645=CARTESIAN_POINT('Ctrl Pts',(-0.777456882345046,5.52890159042847,
-8.90837638241207));
#30646=CARTESIAN_POINT('Ctrl Pts',(-0.71820831960021,9.10409989696232,-5.20031610898184));
#30647=CARTESIAN_POINT('Ctrl Pts',(-0.658959756855376,10.4819698768157,
-0.237128802336295));
#30648=CARTESIAN_POINT('Ctrl Pts',(-0.599711194110542,9.32995446540496,
4.78329094252682));
#30649=CARTESIAN_POINT('Ctrl Pts',(-0.540462631365705,5.92609939215782,
8.64923514311966));
#30650=CARTESIAN_POINT('Ctrl Pts',(-0.481214068620872,1.09194519994383,
10.4276353143587));
#30651=CARTESIAN_POINT('Ctrl Pts',(-0.421965505876034,-4.0057564209339,
9.68926406183886));
#30652=CARTESIAN_POINT('Ctrl Pts',(-0.362716943131203,-8.13664505080342,
6.61233165305132));
#30653=CARTESIAN_POINT('Ctrl Pts',(-0.303468380386365,-10.3037062996053,
1.93947391141822));
#30654=CARTESIAN_POINT('Ctrl Pts',(-0.244219817641532,-9.98390712597543,
-3.20148732097496));
#30655=CARTESIAN_POINT('Ctrl Pts',(-0.184971254896697,-7.25443294882962,
-7.56975066843671));
#30656=CARTESIAN_POINT('Ctrl Pts',(-0.125722692151862,-2.7740584993699,
-10.1110099362393));
#30657=CARTESIAN_POINT('Ctrl Pts',(-0.0664741294070278,2.37585137208773,
-10.211917205029));
#30658=CARTESIAN_POINT('Ctrl Pts',(-0.00722556666219231,6.95233546092519,
-7.848117856984));
#30659=CARTESIAN_POINT('Ctrl Pts',(0.0520229960826416,9.85083230810637,
-3.59012893818949));
#30660=CARTESIAN_POINT('Ctrl Pts',(0.111271558827477,10.3717725107696,1.53435894975116));
#30661=CARTESIAN_POINT('Ctrl Pts',(0.170520121572311,8.38942417794793,6.28851998843207));
#30662=CARTESIAN_POINT('Ctrl Pts',(0.229768684317148,4.38223859253949,9.52491003146027));
#30663=CARTESIAN_POINT('Ctrl Pts',(0.289017247061982,-0.682625920371043,
10.4624058141013));
#30664=CARTESIAN_POINT('Ctrl Pts',(0.348265809806817,-5.58273513680522,
8.8747398847227));
#30665=CARTESIAN_POINT('Ctrl Pts',(0.407514372551651,-9.13541725268214,
5.14509959176606));
#30666=CARTESIAN_POINT('Ctrl Pts',(0.466762935296485,-10.4832142945652,
0.173665725238765));
#30667=CARTESIAN_POINT('Ctrl Pts',(0.52601149804132,-9.30082196402671,-4.8396961877274));
#30668=CARTESIAN_POINT('Ctrl Pts',(0.585260060786157,-5.87362828986304,
-8.68494410471449));
#30669=CARTESIAN_POINT('Ctrl Pts',(0.644508623530991,-1.02878615726,-10.4340771460299));
#30670=CARTESIAN_POINT('Ctrl Pts',(0.703757186275826,4.0643334282463,-9.66479182544668));
#30671=CARTESIAN_POINT('Ctrl Pts',(0.763005749020661,8.1765526549945,-6.56302991227287));
#30672=CARTESIAN_POINT('Ctrl Pts',(0.822254311765496,10.3152148975558,-1.8768974633799));
#30673=CARTESIAN_POINT('Ctrl Pts',(0.88150287451033,9.96442833619652,3.26156383705692));
#30674=CARTESIAN_POINT('Ctrl Pts',(0.940751437255166,7.20829597612923,7.61418408655239));
#30675=CARTESIAN_POINT('Ctrl Pts',(0.980250479085055,4.21155540437341,9.28866001522528));
#30676=CARTESIAN_POINT('Ctrl Pts',(1.,2.60344811511698,9.71940883564396));
#30677=CARTESIAN_POINT('Ctrl Pts',(1.,2.60344811511698,9.71940883564396));
#30678=CARTESIAN_POINT('Ctrl Pts',(1.,2.84069167774707,9.6506072019626));
#30679=CARTESIAN_POINT('Ctrl Pts',(1.00000000000001,3.07490714309636,9.57303457599562));
#30680=CARTESIAN_POINT('Ctrl Pts',(1.,3.30569472464045,9.48703944558796));
#30681=CARTESIAN_POINT('Ctrl Pts',(1.,3.53907106298549,9.40007970314528));
#30682=CARTESIAN_POINT('Ctrl Pts',(1.,3.76894275222114,9.30450718872403));
#30683=CARTESIAN_POINT('Ctrl Pts',(1.,3.99488366234361,9.2006301234426));
#30684=CARTESIAN_POINT('Ctrl Pts',(1.,4.22183130088218,9.09629021151094));
#30685=CARTESIAN_POINT('Ctrl Pts',(1.,4.44481362873405,8.98357126478796));
#30686=CARTESIAN_POINT('Ctrl Pts',(1.,4.66337739592737,8.86273774043803));
#30687=CARTESIAN_POINT('Ctrl Pts',(1.,4.88031644999598,8.74280244279529));
#30688=CARTESIAN_POINT('Ctrl Pts',(0.999999999999998,5.09290290626542,8.61487237722491));
#30689=CARTESIAN_POINT('Ctrl Pts',(0.999999999999998,5.30066443456372,8.47916440146929));
#30690=CARTESIAN_POINT('Ctrl Pts',(0.999999999999998,5.43935724551385,8.38857149536169));
#30691=CARTESIAN_POINT('Ctrl Pts',(0.999999999999999,5.57589930057551,8.29451164480296));
#30692=CARTESIAN_POINT('Ctrl Pts',(0.999999999999998,5.71014105120108,8.19704013131701));
#30693=CARTESIAN_POINT('Ctrl Pts',(0.999999999999998,5.81242655791967,8.12277170810978));
#30694=CARTESIAN_POINT('Ctrl Pts',(1.,5.9133764403282,8.04652243031488));
#30695=CARTESIAN_POINT('Ctrl Pts',(1.,6.01292125894988,7.96831413748024));
#30696=CARTESIAN_POINT('Ctrl Pts',(1.,6.03974575183923,7.94723923047776));
#30697=CARTESIAN_POINT('Ctrl Pts',(1.,6.06647063088991,7.92602003751734));
#30698=CARTESIAN_POINT('Ctrl Pts',(1.,6.09307495250317,7.90467285051554));
#30699=CARTESIAN_POINT('Ctrl Pts',(1.,6.28715174484022,7.74894651255607));
#30700=CARTESIAN_POINT('Ctrl Pts',(0.999999999999995,6.47502692283882,7.58624843803383));
#30701=CARTESIAN_POINT('Ctrl Pts',(0.999999999999996,6.65627725204656,7.41686189931922));
#30702=CARTESIAN_POINT('Ctrl Pts',(0.999999999999996,6.72100528412185,7.35637065850897));
#30703=CARTESIAN_POINT('Ctrl Pts',(0.999999999999999,6.78488816611234,7.29502599747633));
#30704=CARTESIAN_POINT('Ctrl Pts',(0.999999999999999,6.84790570190959,7.23283949466907));
#30705=CARTESIAN_POINT('Ctrl Pts',(1.,7.02385871161102,7.05920683523047));
#30706=CARTESIAN_POINT('Ctrl Pts',(1.,7.19306826910953,6.87901391023897));
#30707=CARTESIAN_POINT('Ctrl Pts',(1.,7.35530118582863,6.69274096896221));
#30708=CARTESIAN_POINT('Ctrl Pts',(1.,7.51824283801115,6.50565427026784));
#30709=CARTESIAN_POINT('Ctrl Pts',(1.,7.67414712093029,6.31243376066224));
#30710=CARTESIAN_POINT('Ctrl Pts',(1.,7.82273682237407,6.1135329641478));
#30711=CARTESIAN_POINT('Ctrl Pts',(1.,7.97083959347484,5.91528396807531));
#30712=CARTESIAN_POINT('Ctrl Pts',(1.,8.11167595875326,5.71139127016028));
#30713=CARTESIAN_POINT('Ctrl Pts',(1.,8.24492584265527,5.50227978289586));
#30714=CARTESIAN_POINT('Ctrl Pts',(1.,8.30521405441425,5.40766838620072));
#30715=CARTESIAN_POINT('Ctrl Pts',(0.999999999999997,8.36394861758055,5.3119883953279));
#30716=CARTESIAN_POINT('Ctrl Pts',(0.999999999999997,8.42109653790941,5.21527801938325));
#30717=CARTESIAN_POINT('Ctrl Pts',(0.999999999999997,8.45087438326695,5.16488551861022));
#30718=CARTESIAN_POINT('Ctrl Pts',(0.999999999999998,8.48022140378265,5.11421324826767));
#30719=CARTESIAN_POINT('Ctrl Pts',(0.999999999999998,8.50913269400644,5.06326655825364));
#30720=CARTESIAN_POINT('Ctrl Pts',(0.999999999999998,8.52853358179415,5.0290788409824));
#30721=CARTESIAN_POINT('Ctrl Pts',(0.999999999999996,8.54774115151347,4.99476217267899));
#30722=CARTESIAN_POINT('Ctrl Pts',(0.999999999999996,8.56673757646602,4.96034807967986));
#30723=CARTESIAN_POINT('Ctrl Pts',(0.999999999999996,8.68625359767795,4.74383178889639));
#30724=CARTESIAN_POINT('Ctrl Pts',(1.,8.79751973028822,4.52328346537184));
#30725=CARTESIAN_POINT('Ctrl Pts',(1.,8.90031168588408,4.29917497997117));
#30726=CARTESIAN_POINT('Ctrl Pts',(1.,9.00301015821637,4.07527030811298));
#30727=CARTESIAN_POINT('Ctrl Pts',(0.999999999999998,9.09725016618283,3.84781136171468));
#30728=CARTESIAN_POINT('Ctrl Pts',(0.999999999999998,9.18276364450296,3.61724215327469));
#30729=CARTESIAN_POINT('Ctrl Pts',(0.999999999999999,9.25013088715846,3.43560047386934));
#30730=CARTESIAN_POINT('Ctrl Pts',(0.999999999999997,9.31208142209733,3.25202787668663));
#30731=CARTESIAN_POINT('Ctrl Pts',(0.999999999999997,9.36846285698885,3.06673337277954));
#30732=CARTESIAN_POINT('Ctrl Pts',(0.999999999999998,9.44021348938853,2.83092884135711));
#30733=CARTESIAN_POINT('Ctrl Pts',(0.999999999999998,9.50294665239736,2.59233553672004));
#30734=CARTESIAN_POINT('Ctrl Pts',(0.999999999999998,9.55662998734371,2.35147826686192));
#30735=CARTESIAN_POINT('Ctrl Pts',(0.999999999999999,9.5940332087379,2.18366384553536));
#30736=CARTESIAN_POINT('Ctrl Pts',(0.999999999999998,9.62704217123799,2.01475016264279));
#30737=CARTESIAN_POINT('Ctrl Pts',(0.999999999999998,9.6556309798987,1.84491423498701));
#30738=CARTESIAN_POINT('Ctrl Pts',(0.999999999999998,9.66985502089958,1.76041427463296));
#30739=CARTESIAN_POINT('Ctrl Pts',(1.,9.68298468440151,1.67568602475725));
#30740=CARTESIAN_POINT('Ctrl Pts',(1.,9.69501564091497,1.59075139934658));
#30741=CARTESIAN_POINT('Ctrl Pts',(1.,9.70329996440281,1.53226677998714));
#30742=CARTESIAN_POINT('Ctrl Pts',(0.999999999999997,9.71106332257942,1.47368430996418));
#30743=CARTESIAN_POINT('Ctrl Pts',(0.999999999999997,9.71830409201168,1.41501118134328));
#30744=CARTESIAN_POINT('Ctrl Pts',(0.999999999999997,9.7217772471656,1.38686764204501));
#30745=CARTESIAN_POINT('Ctrl Pts',(1.,9.72513022957085,1.35870230879726));
#30746=CARTESIAN_POINT('Ctrl Pts',(1.,9.7283610524273,1.33053267129302));
#30747=CARTESIAN_POINT('Ctrl Pts',(1.,9.75621798311309,1.08764729061324));
#30748=CARTESIAN_POINT('Ctrl Pts',(0.999999999999999,9.77503411297353,0.844154061252829));
#30749=CARTESIAN_POINT('Ctrl Pts',(0.999999999999999,9.78485426406749,0.600570610607425));
#30750=CARTESIAN_POINT('Ctrl Pts',(0.999999999999999,9.79474459297459,0.355246437877215));
#30751=CARTESIAN_POINT('Ctrl Pts',(0.999999999999998,9.79550996768915,0.109830095075824));
#30752=CARTESIAN_POINT('Ctrl Pts',(0.999999999999997,9.78714427532281,-0.135157539340118));
#30753=CARTESIAN_POINT('Ctrl Pts',(0.999999999999997,9.77880542326125,-0.379359160777594));
#30754=CARTESIAN_POINT('Ctrl Pts',(0.999999999999999,9.76139398474161,-0.623135475248794));
#30755=CARTESIAN_POINT('Ctrl Pts',(0.999999999999998,9.73485233230931,-0.865968606386387));
#30756=CARTESIAN_POINT('Ctrl Pts',(0.999999999999998,9.70865279306758,-1.10567169814608));
#30757=CARTESIAN_POINT('Ctrl Pts',(0.999999999999997,9.67355680745553,-1.3444563628419));
#30758=CARTESIAN_POINT('Ctrl Pts',(0.999999999999997,9.62945950993569,-1.58181327268759));
#30759=CARTESIAN_POINT('Ctrl Pts',(0.999999999999997,9.6192529840039,-1.63675064054647));
#30760=CARTESIAN_POINT('Ctrl Pts',(0.999999999999998,9.60856403800696,-1.69161145235431));
#30761=CARTESIAN_POINT('Ctrl Pts',(0.999999999999998,9.59739099453272,-1.74638925350567));
#30762=CARTESIAN_POINT('Ctrl Pts',(0.999999999999999,9.55734323773339,-1.94273039041888));
#30763=CARTESIAN_POINT('Ctrl Pts',(0.999999999999998,9.51107764815899,-2.13800595497268));
#30764=CARTESIAN_POINT('Ctrl Pts',(0.999999999999998,9.45868910149449,-2.33194450538573));
#30765=CARTESIAN_POINT('Ctrl Pts',(0.999999999999998,9.44806060011906,-2.37129043653008));
#30766=CARTESIAN_POINT('Ctrl Pts',(0.999999999999997,9.43717863629369,-2.41058591625719));
#30767=CARTESIAN_POINT('Ctrl Pts',(0.999999999999997,9.42605224796243,-2.44979991766584));
#30768=CARTESIAN_POINT('Ctrl Pts',(0.999999999999997,9.35956117629125,-2.68414199710326));
#30769=CARTESIAN_POINT('Ctrl Pts',(0.999999999999997,9.28429949892928,-2.91575317404239));
#30770=CARTESIAN_POINT('Ctrl Pts',(0.999999999999997,9.2005384559038,-3.14417935336596));
#30771=CARTESIAN_POINT('Ctrl Pts',(0.999999999999997,9.11644482312329,-3.3735125439239));
#30772=CARTESIAN_POINT('Ctrl Pts',(0.999999999999997,9.02378391757509,-3.59963600047152));
#30773=CARTESIAN_POINT('Ctrl Pts',(0.999999999999997,8.92278109951216,-3.82207197411459));
#30774=CARTESIAN_POINT('Ctrl Pts',(0.999999999999997,8.83217822944176,-4.02160440306533));
#30775=CARTESIAN_POINT('Ctrl Pts',(0.999999999999999,8.73486209429878,-4.21816969086207));
#30776=CARTESIAN_POINT('Ctrl Pts',(0.999999999999998,8.6309646900063,-4.41140453007061));
#30777=CARTESIAN_POINT('Ctrl Pts',(0.999999999999998,8.6132277511296,-4.4443927895486));
#30778=CARTESIAN_POINT('Ctrl Pts',(0.999999999999999,8.59529894366689,-4.47728393785859));
#30779=CARTESIAN_POINT('Ctrl Pts',(0.999999999999999,8.57717884575786,-4.51007610455165));
#30780=CARTESIAN_POINT('Ctrl Pts',(0.999999999999999,8.56101090653111,-4.5393354253825));
#30781=CARTESIAN_POINT('Ctrl Pts',(0.999999999999998,8.54469196169516,-4.56851353632572));
#30782=CARTESIAN_POINT('Ctrl Pts',(0.999999999999998,8.52822781333363,-4.59759993645712));
#30783=CARTESIAN_POINT('Ctrl Pts',(0.999999999999998,8.40828069815436,-4.80950459803457));
#30784=CARTESIAN_POINT('Ctrl Pts',(0.999999999999999,8.28055247410411,-5.01668529771194));
#30785=CARTESIAN_POINT('Ctrl Pts',(0.999999999999999,8.14527406560948,-5.21867494622436));
#30786=CARTESIAN_POINT('Ctrl Pts',(0.999999999999999,8.01107412784125,-5.41905428659241));
#30787=CARTESIAN_POINT('Ctrl Pts',(1.,7.86944355538485,-5.61432554891969));
#30788=CARTESIAN_POINT('Ctrl Pts',(1.,7.72056576365074,-5.80400382354972));
#30789=CARTESIAN_POINT('Ctrl Pts',(1.,7.65750044054917,-5.88435242044626));
#30790=CARTESIAN_POINT('Ctrl Pts',(1.,7.59313418212457,-5.96369700362708));
#30791=CARTESIAN_POINT('Ctrl Pts',(1.,7.52747886047206,-6.04199877428964));
#30792=CARTESIAN_POINT('Ctrl Pts',(1.,7.42746573325124,-6.1612763096635));
#30793=CARTESIAN_POINT('Ctrl Pts',(1.,7.32446160350885,-6.27813437307676));
#30794=CARTESIAN_POINT('Ctrl Pts',(1.,7.21857426272793,-6.39248696093098));
#30795=CARTESIAN_POINT('Ctrl Pts',(-8.,7.21801009705396,-6.39216838336781));
#30796=CARTESIAN_POINT('Ctrl Pts',(-8.,7.380337662993,-6.21660080725665));
#30797=CARTESIAN_POINT('Ctrl Pts',(-8.,7.53570853367131,-6.03520943062631));
#30798=CARTESIAN_POINT('Ctrl Pts',(-8.,7.68398049959171,-5.84850779751532));
#30799=CARTESIAN_POINT('Ctrl Pts',(-8.,7.83425278465447,-5.65928739527419));
#30800=CARTESIAN_POINT('Ctrl Pts',(-8.,7.97723370551244,-5.46461203049959));
#30801=CARTESIAN_POINT('Ctrl Pts',(-8.,8.1127416114141,-5.26497403764809));
#30802=CARTESIAN_POINT('Ctrl Pts',(-8.,8.24926768438102,-5.06383602287576));
#30803=CARTESIAN_POINT('Ctrl Pts',(-8.,8.37820838989442,-4.85765999894323));
#30804=CARTESIAN_POINT('Ctrl Pts',(-8.,8.49933848010934,-4.64691438626471));
#30805=CARTESIAN_POINT('Ctrl Pts',(-8.,8.6201424258609,-4.43673620909814));
#30806=CARTESIAN_POINT('Ctrl Pts',(-8.,8.733178071977,-4.22201244059188));
#30807=CARTESIAN_POINT('Ctrl Pts',(-8.,8.83817785999191,-4.00318131294289));
#30808=CARTESIAN_POINT('Ctrl Pts',(-8.,8.90711924309347,-3.85949987423702));
#30809=CARTESIAN_POINT('Ctrl Pts',(-8.,8.97259541777826,-3.71404720995258));
#30810=CARTESIAN_POINT('Ctrl Pts',(-8.,9.03451925692504,-3.56694295599801));
#30811=CARTESIAN_POINT('Ctrl Pts',(-8.,9.0602105812632,-3.50591148327374));
#30812=CARTESIAN_POINT('Ctrl Pts',(-8.,9.08529032912163,-3.44459568829976));
#30813=CARTESIAN_POINT('Ctrl Pts',(-8.,9.10975179059862,-3.38300398939247));
#30814=CARTESIAN_POINT('Ctrl Pts',(-8.,9.12543389087233,-3.34351791047601));
#30815=CARTESIAN_POINT('Ctrl Pts',(-8.,9.1408618685122,-3.30391843322633));
#30816=CARTESIAN_POINT('Ctrl Pts',(-8.,9.15603389139516,-3.26420776351618));
#30817=CARTESIAN_POINT('Ctrl Pts',(-8.,9.16539707181774,-3.23970093485752));
#30818=CARTESIAN_POINT('Ctrl Pts',(-8.,9.17466357769889,-3.21514958524345));
#30819=CARTESIAN_POINT('Ctrl Pts',(-8.,9.18383032373706,-3.19056134096833));
#30820=CARTESIAN_POINT('Ctrl Pts',(-8.,9.26956766576029,-2.96058543671737));
#30821=CARTESIAN_POINT('Ctrl Pts',(-8.,9.34642836267942,-2.72780037578161));
#30822=CARTESIAN_POINT('Ctrl Pts',(-8.,9.41421809880825,-2.49269184582416));
#30823=CARTESIAN_POINT('Ctrl Pts',(-8.,9.44158158155583,-2.39778974750246));
#30824=CARTESIAN_POINT('Ctrl Pts',(-8.,9.46746660052344,-2.30250872996448));
#30825=CARTESIAN_POINT('Ctrl Pts',(-8.,9.49185833340935,-2.20687947232321));
#30826=CARTESIAN_POINT('Ctrl Pts',(-8.,9.55185317751319,-1.97166607314452));
#30827=CARTESIAN_POINT('Ctrl Pts',(-8.,9.60281745079054,-1.73434714094384));
#30828=CARTESIAN_POINT('Ctrl Pts',(-8.,9.64482582839825,-1.49544885170401));
#30829=CARTESIAN_POINT('Ctrl Pts',(-8.,9.687149082017,-1.25475988773113));
#30830=CARTESIAN_POINT('Ctrl Pts',(-8.,9.72038175363905,-1.01246716488642));
#30831=CARTESIAN_POINT('Ctrl Pts',(-8.,9.74454885870802,-0.769095294744196));
#30832=CARTESIAN_POINT('Ctrl Pts',(-8.,9.76872028978328,-0.525679860085804));
#30833=CARTESIAN_POINT('Ctrl Pts',(-8.,9.78382293411453,-0.281184228473798));
#30834=CARTESIAN_POINT('Ctrl Pts',(-8.,9.78982997440973,-0.0361296562227952));
#30835=CARTESIAN_POINT('Ctrl Pts',(-8.,9.79255533923483,0.0750504056083886));
#30836=CARTESIAN_POINT('Ctrl Pts',(-8.,9.79340776314294,0.186345508045464));
#30837=CARTESIAN_POINT('Ctrl Pts',(-8.,9.79238119762556,0.297706651553354));
#30838=CARTESIAN_POINT('Ctrl Pts',(-8.,9.79184842307034,0.355501680410697));
#30839=CARTESIAN_POINT('Ctrl Pts',(-8.,9.79080951024432,0.413314491676565));
#30840=CARTESIAN_POINT('Ctrl Pts',(-8.,9.78926337738701,0.471138189497998));
#30841=CARTESIAN_POINT('Ctrl Pts',(-8.,9.78827687496122,0.50803231402231));
#30842=CARTESIAN_POINT('Ctrl Pts',(-8.,9.78708363293494,0.544935840717242));
#30843=CARTESIAN_POINT('Ctrl Pts',(-8.,9.78568466161457,0.581816587647619));
#30844=CARTESIAN_POINT('Ctrl Pts',(-8.,9.77634732562296,0.827974547211403));
#30845=CARTESIAN_POINT('Ctrl Pts',(-8.,9.75784567918533,1.07334629644098));
#30846=CARTESIAN_POINT('Ctrl Pts',(-8.,9.73025873568655,1.31740270617224));
#30847=CARTESIAN_POINT('Ctrl Pts',(-8.,9.70256576677612,1.56239710242996));
#30848=CARTESIAN_POINT('Ctrl Pts',(-8.,9.66571755991781,1.80606669459938));
#30849=CARTESIAN_POINT('Ctrl Pts',(-8.,9.61974208798732,2.04788261285709));
#30850=CARTESIAN_POINT('Ctrl Pts',(-8.,9.58407745535832,2.2354668947878));
#30851=CARTESIAN_POINT('Ctrl Pts',(-8.,9.54291936511459,2.42193593333913));
#30852=CARTESIAN_POINT('Ctrl Pts',(-8.,9.49625929589928,2.60704160924379));
#30853=CARTESIAN_POINT('Ctrl Pts',(-8.,9.43617821052004,2.84538994659596));
#30854=CARTESIAN_POINT('Ctrl Pts',(-8.,9.36697643674185,3.08147866016247));
#30855=CARTESIAN_POINT('Ctrl Pts',(-8.,9.28891878956949,3.31486179503419));
#30856=CARTESIAN_POINT('Ctrl Pts',(-8.,9.23376423793927,3.47976738248396));
#30857=CARTESIAN_POINT('Ctrl Pts',(-8.,9.17418715731129,3.64332194306396));
#30858=CARTESIAN_POINT('Ctrl Pts',(-8.,9.11026643845191,3.8053622791706));
#30859=CARTESIAN_POINT('Ctrl Pts',(-8.,9.07823135006152,3.88657188667525));
#30860=CARTESIAN_POINT('Ctrl Pts',(-8.,9.04510508571049,3.96740107672111));
#30861=CARTESIAN_POINT('Ctrl Pts',(-8.,9.01089650850777,4.04782870220661));
#30862=CARTESIAN_POINT('Ctrl Pts',(-8.,8.98491018599784,4.10892502323126));
#30863=CARTESIAN_POINT('Ctrl Pts',(-8.,8.95829929144517,4.16978960999898));
#30864=CARTESIAN_POINT('Ctrl Pts',(-8.,8.93106744624091,4.2304130132153));
#30865=CARTESIAN_POINT('Ctrl Pts',(-8.,8.91985556199095,4.25537285617128));
#30866=CARTESIAN_POINT('Ctrl Pts',(-8.,8.90854177922313,4.2802842982631));
#30867=CARTESIAN_POINT('Ctrl Pts',(-8.,8.89712828878493,4.30514299630826));
#30868=CARTESIAN_POINT('Ctrl Pts',(-8.,8.79449435935336,4.52868073655892));
#30869=CARTESIAN_POINT('Ctrl Pts',(-8.,8.68375805043763,4.74805239503432));
#30870=CARTESIAN_POINT('Ctrl Pts',(-8.,8.56525012527811,4.96284306665098));
#30871=CARTESIAN_POINT('Ctrl Pts',(-8.,8.44538164369718,5.18009969003529));
#30872=CARTESIAN_POINT('Ctrl Pts',(-8.,8.31756185464637,5.39267013945067));
#30873=CARTESIAN_POINT('Ctrl Pts',(-8.,8.18208202554571,5.60011073616086));
#30874=CARTESIAN_POINT('Ctrl Pts',(-8.,8.04666337133259,5.80745766464561));
#30875=CARTESIAN_POINT('Ctrl Pts',(-8.,7.9035912805775,6.00967995783845));
#30876=CARTESIAN_POINT('Ctrl Pts',(-8.,7.75311010158105,6.20631140538698));
#30877=CARTESIAN_POINT('Ctrl Pts',(-8.,7.60409269401218,6.40103016527181));
#30878=CARTESIAN_POINT('Ctrl Pts',(-8.,7.44780928129002,6.59026684301417));
#30879=CARTESIAN_POINT('Ctrl Pts',(-8.,7.2844565981824,6.77353780787826));
#30880=CARTESIAN_POINT('Ctrl Pts',(-8.,7.25089455072778,6.8111922173609));
#30881=CARTESIAN_POINT('Ctrl Pts',(-8.,7.21703396184226,6.84859467696372));
#30882=CARTESIAN_POINT('Ctrl Pts',(-8.,7.18287634384795,6.88574079722686));
#30883=CARTESIAN_POINT('Ctrl Pts',(-8.,7.04310058845776,7.03774574735134));
#30884=CARTESIAN_POINT('Ctrl Pts',(-8.,6.89835220047973,7.18545984496082));
#30885=CARTESIAN_POINT('Ctrl Pts',(-8.,6.748868793449,7.32870634277334));
#30886=CARTESIAN_POINT('Ctrl Pts',(-8.,6.72044536021718,7.35594386262349));
#30887=CARTESIAN_POINT('Ctrl Pts',(-8.,6.6918476905919,7.38302252032495));
#30888=CARTESIAN_POINT('Ctrl Pts',(-8.,6.66309763711236,7.40992229604933));
#30889=CARTESIAN_POINT('Ctrl Pts',(-8.,6.48228035952991,7.57910264966232));
#30890=CARTESIAN_POINT('Ctrl Pts',(-8.,6.29529505695125,7.74135050059987));
#30891=CARTESIAN_POINT('Ctrl Pts',(-8.,6.10262671834098,7.89643860443478));
#30892=CARTESIAN_POINT('Ctrl Pts',(-8.,5.90856001007317,8.0526523239272));
#30893=CARTESIAN_POINT('Ctrl Pts',(-8.,5.70872697509029,8.20160239784391));
#30894=CARTESIAN_POINT('Ctrl Pts',(-8.,5.50358539266632,8.34301978271322));
#30895=CARTESIAN_POINT('Ctrl Pts',(-8.,5.31584799310374,8.47243933663592));
#30896=CARTESIAN_POINT('Ctrl Pts',(-8.,5.12366384911883,8.5955499246735));
#30897=CARTESIAN_POINT('Ctrl Pts',(-8.,4.92736179531277,8.71211422557509));
#30898=CARTESIAN_POINT('Ctrl Pts',(-8.,4.89295954023047,8.73254230941505));
#30899=CARTESIAN_POINT('Ctrl Pts',(-8.,4.85843076693046,8.75276925692888));
#30900=CARTESIAN_POINT('Ctrl Pts',(-8.,4.82377719165751,8.77279368760958));
#30901=CARTESIAN_POINT('Ctrl Pts',(-8.,4.79450813280393,8.78970669688745));
#30902=CARTESIAN_POINT('Ctrl Pts',(-8.,4.76515157202874,8.80647430503471));
#30903=CARTESIAN_POINT('Ctrl Pts',(-8.,4.73571877014772,8.82309008094362));
#30904=CARTESIAN_POINT('Ctrl Pts',(-8.,4.5175174124504,8.94627185878366));
#30905=CARTESIAN_POINT('Ctrl Pts',(-8.,4.29497552947991,9.0612009825643));
#30906=CARTESIAN_POINT('Ctrl Pts',(-8.,4.06855852697811,9.16761501762388));
#30907=CARTESIAN_POINT('Ctrl Pts',(-8.,3.84298108906434,9.27363446458045));
#30908=CARTESIAN_POINT('Ctrl Pts',(-8.,3.61355665285897,9.37120219380835));
#30909=CARTESIAN_POINT('Ctrl Pts',(-8.,3.38071837058219,9.46001495319009));
#30910=CARTESIAN_POINT('Ctrl Pts',(-8.,3.27719791908491,9.49950131625726));
#30911=CARTESIAN_POINT('Ctrl Pts',(-8.,3.17300234029469,9.53725646338326));
#30912=CARTESIAN_POINT('Ctrl Pts',(-8.,3.06816841590428,9.57325067970064));
#30913=CARTESIAN_POINT('Ctrl Pts',(-8.,2.9146850890607,9.62594843092614));
#30914=CARTESIAN_POINT('Ctrl Pts',(-8.,2.75983355042631,9.67487206864313));
#30915=CARTESIAN_POINT('Ctrl Pts',(-8.,2.6037558201701,9.72001092048762));
#30916=CARTESIAN_POINT('Ctrl Pts',(0.711515937838069,-9.64233463315361,
5.55577575209881E-5));
#30917=CARTESIAN_POINT('Ctrl Pts',(0.710856866388953,-9.64235142088166,
0.053277087912501));
#30918=CARTESIAN_POINT('Ctrl Pts',(0.710197794939836,-9.64191990087921,
0.10649834290957));
#30919=CARTESIAN_POINT('Ctrl Pts',(0.70953872349072,-9.64103837930507,0.15971214088109));
#30920=CARTESIAN_POINT('Ctrl Pts',(0.689789202575776,-9.61462299021662,
1.75429952197757));
#30921=CARTESIAN_POINT('Ctrl Pts',(0.670039681660832,-9.18413243182588,
3.34219092899087));
#30922=CARTESIAN_POINT('Ctrl Pts',(0.650290160745888,-8.40151830542192,
4.73176597520196));
#30923=CARTESIAN_POINT('Ctrl Pts',(0.630540639830942,-7.61890417901792,
6.12134102141313));
#30924=CARTESIAN_POINT('Ctrl Pts',(0.610791118915997,-6.48416648460066,
7.31259970682207));
#30925=CARTESIAN_POINT('Ctrl Pts',(0.591041598001052,-5.13424259119184,
8.16178176230046));
#30926=CARTESIAN_POINT('Ctrl Pts',(0.571292077086108,-3.78431869778303,
9.01096381777884));
#30927=CARTESIAN_POINT('Ctrl Pts',(0.551542556171163,-2.21920860538266,
9.51806924332668));
#30928=CARTESIAN_POINT('Ctrl Pts',(0.531793035256218,-0.627786836456111,
9.62190242474063));
#30929=CARTESIAN_POINT('Ctrl Pts',(0.512043514341272,0.963634932470433,
9.72573560615459));
#30930=CARTESIAN_POINT('Ctrl Pts',(0.492293993426328,2.58136837792315,9.42629654343467));
#30931=CARTESIAN_POINT('Ctrl Pts',(0.472544472511382,4.03018885727291,8.75972049974441));
#30932=CARTESIAN_POINT('Ctrl Pts',(0.452794951596437,5.47900933662266,8.09314445605415));
#30933=CARTESIAN_POINT('Ctrl Pts',(0.433045430681492,6.75891684986946,7.05943143139355));
#30934=CARTESIAN_POINT('Ctrl Pts',(0.413295909766547,7.71545471159267,5.78332802334296));
#30935=CARTESIAN_POINT('Ctrl Pts',(0.393546388851601,8.67199257331588,4.50722461529236));
#30936=CARTESIAN_POINT('Ctrl Pts',(0.373796867936656,9.30516078351549,2.98873082385177));
#30937=CARTESIAN_POINT('Ctrl Pts',(0.354047347021711,9.53854992981817,1.41109525988503));
#30938=CARTESIAN_POINT('Ctrl Pts',(0.334297826106766,9.77193907612084,-0.166540304081665));
#30939=CARTESIAN_POINT('Ctrl Pts',(0.314548305191821,9.60554915852659,-1.8033176405745));
#30940=CARTESIAN_POINT('Ctrl Pts',(0.294798784276877,9.05945975514247,-3.3017137470004));
#30941=CARTESIAN_POINT('Ctrl Pts',(0.275049263361932,8.51337035175834,-4.80010985342633));
#30942=CARTESIAN_POINT('Ctrl Pts',(0.255299742446987,7.58758146258432,-6.16012472978531));
#30943=CARTESIAN_POINT('Ctrl Pts',(0.235550221532042,6.39381540689866,-7.2176345921584));
#30944=CARTESIAN_POINT('Ctrl Pts',(0.215800700617097,5.200049351213,-8.27514445453149));
#30945=CARTESIAN_POINT('Ctrl Pts',(0.196051179702152,3.7383061290157,-9.03014930291869));
#30946=CARTESIAN_POINT('Ctrl Pts',(0.176301658787207,2.18498591945131,-9.39153667969154));
#30947=CARTESIAN_POINT('Ctrl Pts',(0.156552137872262,0.631665709886971,
-9.75292405646439));
#30948=CARTESIAN_POINT('Ctrl Pts',(0.136802616957318,-1.01323148704445,
-9.7206939616229));
#30949=CARTESIAN_POINT('Ctrl Pts',(0.117053096042373,-2.55120283805044,
-9.29873586542844));
#30950=CARTESIAN_POINT('Ctrl Pts',(0.0973035751274285,-4.08917418905644,
-8.87677776923399));
#30951=CARTESIAN_POINT('Ctrl Pts',(0.0775540542124838,-5.52021969413699,
-8.06509167168657));
#30952=CARTESIAN_POINT('Ctrl Pts',(0.0578045332975393,-6.67164370855832,
-6.96163018734359));
#30953=CARTESIAN_POINT('Ctrl Pts',(0.0380550123825936,-7.8230677229797,
-5.85816870300055));
#30954=CARTESIAN_POINT('Ctrl Pts',(0.0183054914676481,-8.69487024674182,
-4.46293183186192));
#30955=CARTESIAN_POINT('Ctrl Pts',(-0.00144402944729742,-9.1818439329385,
-2.94429390937257));
#30956=CARTESIAN_POINT('Ctrl Pts',(-0.013790707018842,-9.48628205653607,
-1.99489706791769));
#30957=CARTESIAN_POINT('Ctrl Pts',(-0.0261373845903865,-9.6403178056493,
-0.997271483382048));
#30958=CARTESIAN_POINT('Ctrl Pts',(-0.0384840621619312,-9.6409393879154,
0.000166496178767295));
#30959=CARTESIAN_POINT('Ctrl Pts',(-8.,-2.60344811511687,9.71940883564398));
#30960=CARTESIAN_POINT('Ctrl Pts',(-7.98025047908506,-4.2115554043733,9.28866001522532));
#30961=CARTESIAN_POINT('Ctrl Pts',(-7.94075143725516,-7.20829614504029,
7.61418486945486));
#30962=CARTESIAN_POINT('Ctrl Pts',(-7.88150287451034,-9.96442823502186,
3.26156338357991));
#30963=CARTESIAN_POINT('Ctrl Pts',(-7.82225431176549,-10.3152149209058,
-1.87689719875276));
#30964=CARTESIAN_POINT('Ctrl Pts',(-7.76300574902067,-8.17655263057037,
-6.56303005806257));
#30965=CARTESIAN_POINT('Ctrl Pts',(-7.70375718627582,-4.06433342707358,
-9.66479172255802));
#30966=CARTESIAN_POINT('Ctrl Pts',(-7.644508623531,1.02878615653537,-10.4340771844272));
#30967=CARTESIAN_POINT('Ctrl Pts',(-7.58526006078616,5.87362828262073,-8.68494406353048));
#30968=CARTESIAN_POINT('Ctrl Pts',(-7.52601149804132,9.30082195115954,-4.83969619824767));
#30969=CARTESIAN_POINT('Ctrl Pts',(-7.46676293529649,10.483214281353,0.173665734501785));
#30970=CARTESIAN_POINT('Ctrl Pts',(-7.40751437255165,9.13541724029078,5.1450995797055));
#30971=CARTESIAN_POINT('Ctrl Pts',(-7.34826580980682,5.58273512973762,8.87473987601911));
#30972=CARTESIAN_POINT('Ctrl Pts',(-7.28901724706198,0.682625919309218,
10.4624057987323));
#30973=CARTESIAN_POINT('Ctrl Pts',(-7.22976868431715,-4.38223858668436,
9.52491001985317));
#30974=CARTESIAN_POINT('Ctrl Pts',(-7.17052012157231,-8.38942416699272,
6.28851997968158));
#30975=CARTESIAN_POINT('Ctrl Pts',(-7.11127155882747,-10.371772497116,1.53435894800687));
#30976=CARTESIAN_POINT('Ctrl Pts',(-7.05202299608265,-9.85083229519261,
-3.59012893362295));
#30977=CARTESIAN_POINT('Ctrl Pts',(-6.9927744333378,-6.95233545178506,-7.84811784659899));
#30978=CARTESIAN_POINT('Ctrl Pts',(-6.93352587059297,-2.37585136897494,
-10.2119171916642));
#30979=CARTESIAN_POINT('Ctrl Pts',(-6.87427730784814,2.77405849573116,-10.1110099229398));
#30980=CARTESIAN_POINT('Ctrl Pts',(-6.8150287451033,7.25443293930229,-7.56975065851036));
#30981=CARTESIAN_POINT('Ctrl Pts',(-6.75578018235847,9.98390711286757,-3.20148731676458));
#30982=CARTESIAN_POINT('Ctrl Pts',(-6.69653161961363,10.3037062860758,1.93947390886785));
#30983=CARTESIAN_POINT('Ctrl Pts',(-6.63728305686881,8.13664504012033,6.61233164437115));
#30984=CARTESIAN_POINT('Ctrl Pts',(-6.57803449412396,4.00575641567419,9.68926404911563));
#30985=CARTESIAN_POINT('Ctrl Pts',(-6.51878593137913,-1.09194519850991,
10.4276353006677));
#30986=CARTESIAN_POINT('Ctrl Pts',(-6.45953736863429,-5.92609938437677,
8.64923513176283));
#30987=CARTESIAN_POINT('Ctrl Pts',(-6.40028880588946,-9.32995445315455,
4.78329093624652));
#30988=CARTESIAN_POINT('Ctrl Pts',(-6.34104024314462,-10.4819698630527,
-0.237128802024965));
#30989=CARTESIAN_POINT('Ctrl Pts',(-6.28179168039979,-9.10409988500852,
-5.20031610215367));
#30990=CARTESIAN_POINT('Ctrl Pts',(-6.22254311765495,-5.52890158316907,
-8.90837637071521));
#30991=CARTESIAN_POINT('Ctrl Pts',(-6.16329455491012,-0.61927020154201,
-10.4663473426058));
#30992=CARTESIAN_POINT('Ctrl Pts',(-6.10404599216529,4.43982570388255,-9.49820351423256));
#30993=CARTESIAN_POINT('Ctrl Pts',(-6.04479742942044,8.42734343078316,-6.23761212149772));
#30994=CARTESIAN_POINT('Ctrl Pts',(-5.98554886667563,10.3808720045808,-1.47153617119417));
#30995=CARTESIAN_POINT('Ctrl Pts',(-5.92630030393077,9.82891575620613,3.64970373263731));
#30996=CARTESIAN_POINT('Ctrl Pts',(-5.86705174118595,6.90469258895211,7.89006606630713));
#30997=CARTESIAN_POINT('Ctrl Pts',(-5.80780317844112,2.31398105003217,10.2261143147686));
#30998=CARTESIAN_POINT('Ctrl Pts',(-5.74855461569627,-2.83522349381956,
10.094029424304));
#30999=CARTESIAN_POINT('Ctrl Pts',(-5.68930605295145,-7.3001300877402,7.5256908640133));
#31000=CARTESIAN_POINT('Ctrl Pts',(-5.63005749020659,-10.0031071321348,
3.14098232749819));
#31001=CARTESIAN_POINT('Ctrl Pts',(-5.57080892746178,-10.2917751393821,
-2.00182086087136));
#31002=CARTESIAN_POINT('Ctrl Pts',(-5.51156036471693,-8.09646237954581,
-6.66147275121817));
#31003=CARTESIAN_POINT('Ctrl Pts',(-5.4523118019721,-3.94702056424182,-9.71333881546786));
#31004=CARTESIAN_POINT('Ctrl Pts',(-5.39306323922727,1.15505799604341,-10.420833138689));
#31005=CARTESIAN_POINT('Ctrl Pts',(-5.33381467648243,5.97835648115395,-8.61319778380056));
#31006=CARTESIAN_POINT('Ctrl Pts',(-5.27456611373759,9.35874329001436,-4.72671622907851));
#31007=CARTESIAN_POINT('Ctrl Pts',(-5.21531755099276,10.480342084015,0.300586228304444));
#31008=CARTESIAN_POINT('Ctrl Pts',(-5.15606898824793,9.07244836417983,5.25534042264758));
#31009=CARTESIAN_POINT('Ctrl Pts',(-5.09682042550309,5.47486560219418,8.9416871403854));
#31010=CARTESIAN_POINT('Ctrl Pts',(-5.03757186275826,0.555891663852748,
10.4699048102971));
#31011=CARTESIAN_POINT('Ctrl Pts',(-4.97832330001342,-4.49725001357077,
9.47114906408194));
#31012=CARTESIAN_POINT('Ctrl Pts',(-4.91907473726859,-8.464953815877,6.18647550497794));
#31013=CARTESIAN_POINT('Ctrl Pts',(-4.85982617452375,-10.3895909763142,
1.40865951298154));
#31014=CARTESIAN_POINT('Ctrl Pts',(-4.80057761177892,-9.80663893921103,
-3.70914477940301));
#31015=CARTESIAN_POINT('Ctrl Pts',(-4.74132904903408,-6.85679662469408,
-7.93172505361893));
#31016=CARTESIAN_POINT('Ctrl Pts',(-4.68208048628925,-2.25202591260958,
-10.2399365997821));
#31017=CARTESIAN_POINT('Ctrl Pts',(-4.62283192354441,2.89628456575783,-10.0766789168245));
#31018=CARTESIAN_POINT('Ctrl Pts',(-4.56358336079958,7.34555964353492,-7.48135521158391));
#31019=CARTESIAN_POINT('Ctrl Pts',(-4.50433479805474,10.0219404799498,-3.08036220191168));
#31020=CARTESIAN_POINT('Ctrl Pts',(-4.44508623530991,10.2794667393936,2.0640944339644));
#31021=CARTESIAN_POINT('Ctrl Pts',(-4.38583767256508,8.0559829368491,6.71036967683738));
#31022=CARTESIAN_POINT('Ctrl Pts',(-4.32658910982024,3.88814003161556,9.73705753157345));
#31023=CARTESIAN_POINT('Ctrl Pts',(-4.2673405470754,-1.21812845399267,10.4136489929417));
#31024=CARTESIAN_POINT('Ctrl Pts',(-4.20809198433057,-6.03039443657531,
8.57684471224378));
#31025=CARTESIAN_POINT('Ctrl Pts',(-4.14884342158573,-9.3871890747578,4.66996826042431));
#31026=CARTESIAN_POINT('Ctrl Pts',(-4.08959485884091,-10.4783301397828,
-0.364032636370266));
#31027=CARTESIAN_POINT('Ctrl Pts',(-4.03034629609606,-9.04046428560539,
-5.31017210449113));
#31028=CARTESIAN_POINT('Ctrl Pts',(-3.97109773335123,-5.42062893570726,
-8.9746701454703));
#31029=CARTESIAN_POINT('Ctrl Pts',(-3.9118491706064,-0.492492749516077,
-10.4730784953755));
#31030=CARTESIAN_POINT('Ctrl Pts',(-3.85260060786156,4.5545094730156,-9.4437474414998));
#31031=CARTESIAN_POINT('Ctrl Pts',(-3.79335204511673,8.50225391141831,-6.13511211832306));
#31032=CARTESIAN_POINT('Ctrl Pts',(-3.73410348237189,10.3979291094031,-1.34573121924465));
#31033=CARTESIAN_POINT('Ctrl Pts',(-3.67485491962706,9.78400265213786,3.76844986454401));
#31034=CARTESIAN_POINT('Ctrl Pts',(-3.61560635688222,6.80864931915254,7.97309329729851));
#31035=CARTESIAN_POINT('Ctrl Pts',(-3.55635779413739,2.18998822540255,10.2533835318504));
#31036=CARTESIAN_POINT('Ctrl Pts',(-3.49710923139255,-2.95723947210302,
10.0589590407387));
#31037=CARTESIAN_POINT('Ctrl Pts',(-3.43786066864772,-7.39071994205252,
7.43674532418379));
#31038=CARTESIAN_POINT('Ctrl Pts',(-3.37861210590288,-10.040406465639,3.01962916322129));
#31039=CARTESIAN_POINT('Ctrl Pts',(-3.31936354315805,-10.2667815374515,
-2.1262923460494));
#31040=CARTESIAN_POINT('Ctrl Pts',(-3.26011498041321,-8.01520819574961,
-6.75902062856823));
#31041=CARTESIAN_POINT('Ctrl Pts',(-3.20086641766838,-3.82911697615253,
-9.76041932816225));
#31042=CARTESIAN_POINT('Ctrl Pts',(-3.14161785492354,1.28115426048353,-10.4060831266845));
#31043=CARTESIAN_POINT('Ctrl Pts',(-3.08236929217871,6.08221134313651,-8.54017724968541));
#31044=CARTESIAN_POINT('Ctrl Pts',(-3.02312072943387,9.41529076468844,-4.61304911040355));
#31045=CARTESIAN_POINT('Ctrl Pts',(-2.96387216668904,10.4759341041022,0.427465700532903));
#31046=CARTESIAN_POINT('Ctrl Pts',(-2.9046236039442,9.00814882168857,5.36480913779172));
#31047=CARTESIAN_POINT('Ctrl Pts',(-2.84537504119937,5.36619357179512,9.00732417694884));
#31048=CARTESIAN_POINT('Ctrl Pts',(-2.78612647845453,0.429075782469587,
10.4758682815087));
#31049=CARTESIAN_POINT('Ctrl Pts',(-2.7268779157097,-4.61160198332664,9.41599965091337));
#31050=CARTESIAN_POINT('Ctrl Pts',(-2.66762935296486,-8.5392423501426,6.08352384429894));
#31051=CARTESIAN_POINT('Ctrl Pts',(-2.60838079022003,-10.4058860982068,
1.28275359666941));
#31052=CARTESIAN_POINT('Ctrl Pts',(-2.54913222747519,-9.7610077247375,-3.82761681418572));
#31053=CARTESIAN_POINT('Ctrl Pts',(-2.48988366473036,-6.76025243720484,
-8.01416928096036));
#31054=CARTESIAN_POINT('Ctrl Pts',(-2.43063510198552,-2.12787026245138,
-10.2664546180655));
#31055=CARTESIAN_POINT('Ctrl Pts',(-2.37138653924069,3.01808597850499,-10.0408704455826));
#31056=CARTESIAN_POINT('Ctrl Pts',(-2.31213797649586,7.43560932790665,-7.39186283702356));
#31057=CARTESIAN_POINT('Ctrl Pts',(-2.25288941375102,10.0585044123173,-2.95878543764436));
#31058=CARTESIAN_POINT('Ctrl Pts',(-2.19364085100618,10.2537199985417,2.18841231721289));
#31059=CARTESIAN_POINT('Ctrl Pts',(-2.13439228826135,7.97413965087761,6.80742382307171));
#31060=CARTESIAN_POINT('Ctrl Pts',(-2.07514372551652,3.76995356138932,9.78342334888923));
#31061=CARTESIAN_POINT('Ctrl Pts',(-2.01589516277168,-1.34413310525547,
10.3981358172501));
#31062=CARTESIAN_POINT('Ctrl Pts',(-1.95664660002685,-6.1338053014481,8.50319674020009));
#31063=CARTESIAN_POINT('Ctrl Pts',(-1.89739803728201,-9.44304732971672,
4.5559608654325));
#31064=CARTESIAN_POINT('Ctrl Pts',(-1.83814947453718,-10.4731540648018,
-0.490883095603427));
#31065=CARTESIAN_POINT('Ctrl Pts',(-1.77890091179234,-8.97550315697813,
-5.41924951978578));
#31066=CARTESIAN_POINT('Ctrl Pts',(-1.71965234904751,-5.31156150582896,
-9.03964803786181));
#31067=CARTESIAN_POINT('Ctrl Pts',(-1.66040378630267,-0.365643087312114,
-10.4782740664349));
#31068=CARTESIAN_POINT('Ctrl Pts',(-1.60115522355784,4.66852545173299,-9.38790670943975));
#31069=CARTESIAN_POINT('Ctrl Pts',(-1.541906660813,8.57591777620947,-6.03171257391441));
#31070=CARTESIAN_POINT('Ctrl Pts',(-1.48265809806816,10.4134616510556,-1.2197289537503));
#31071=CARTESIAN_POINT('Ctrl Pts',(-1.42340953532333,9.73765499990719,3.88664345951686));
#31072=CARTESIAN_POINT('Ctrl Pts',(-1.3641609725785,6.71160775287686,8.05495149893194));
#31073=CARTESIAN_POINT('Ctrl Pts',(-1.30491240983366,2.06567430073889,10.2791493792964));
#31074=CARTESIAN_POINT('Ctrl Pts',(-1.24566384708883,-3.07882185458713,
10.022413794408));
#31075=CARTESIAN_POINT('Ctrl Pts',(-1.18641528434399,-7.48022615564147,
7.34670939530617));
#31076=CARTESIAN_POINT('Ctrl Pts',(-1.12716672159916,-10.07623365659,2.89783325545567));
#31077=CARTESIAN_POINT('Ctrl Pts',(-1.06791815885432,-10.2402826014452,
-2.25045207039839));
#31078=CARTESIAN_POINT('Ctrl Pts',(-1.00866959610949,-7.93277880763296,
-6.85557748609057));
#31079=CARTESIAN_POINT('Ctrl Pts',(-0.949421033364655,-3.7106519560076,
-9.80606875052385));
#31080=CARTESIAN_POINT('Ctrl Pts',(-0.890172470619817,1.40706267976922,
-10.3898073559533));
#31081=CARTESIAN_POINT('Ctrl Pts',(-0.830923907874984,6.18517442029282,
-8.46590453933774));
#31082=CARTESIAN_POINT('Ctrl Pts',(-0.771675345130147,9.47045775240396,
-4.49870561812545));
#31083=CARTESIAN_POINT('Ctrl Pts',(-0.712426782385315,10.4699901237859,
0.554282496966878));
#31084=CARTESIAN_POINT('Ctrl Pts',(-0.65317821964048,8.94252848812691,5.47349125491902));
#31085=CARTESIAN_POINT('Ctrl Pts',(-0.593929656895644,5.25673474038977,
9.07164054335094));
#31086=CARTESIAN_POINT('Ctrl Pts',(-0.53468109415081,0.302196989220137,
10.4802957619713));
#31087=CARTESIAN_POINT('Ctrl Pts',(-0.475432531405974,-4.72527779166189,
9.35946964684205));
#31088=CARTESIAN_POINT('Ctrl Pts',(-0.41618396866114,-8.61227884524871,
5.97968020636365));
#31089=CARTESIAN_POINT('Ctrl Pts',(-0.356935405916305,-10.4206554902685,
1.15665960068344));
#31090=CARTESIAN_POINT('Ctrl Pts',(-0.29768684317147,-9.71394533364604,
-3.94552763682723));
#31091=CARTESIAN_POINT('Ctrl Pts',(-0.238438280426636,-6.66271704930368,
-8.09543845639));
#31092=CARTESIAN_POINT('Ctrl Pts',(-0.1791897176818,-2.00340262005729,-10.2914673500501));
#31093=CARTESIAN_POINT('Ctrl Pts',(-0.119941154936964,3.13944487393184,
-10.0035897640602));
#31094=CARTESIAN_POINT('Ctrl Pts',(-0.0606925921921299,7.52456878997794,
-7.3012866535828));
#31095=CARTESIAN_POINT('Ctrl Pts',(-0.00144402944729414,10.0935935482191,
-2.83677485203218));
#31096=CARTESIAN_POINT('Ctrl Pts',(0.0578045332975393,10.2264698394132,
2.3124093336654));
#31097=CARTESIAN_POINT('Ctrl Pts',(0.117053096042374,7.89112718079254,6.90347984831441));
#31098=CARTESIAN_POINT('Ctrl Pts',(0.176301658787208,3.65121433633638,9.82835471108965));
#31099=CARTESIAN_POINT('Ctrl Pts',(0.235550221532044,-1.46994068227644,
10.3810980324261));
#31100=CARTESIAN_POINT('Ctrl Pts',(0.294798784276879,-6.23631680707128,
8.42830204429616));
#31101=CARTESIAN_POINT('Ctrl Pts',(0.354047347021714,-9.4975210465794,4.44128540887));
#31102=CARTESIAN_POINT('Ctrl Pts',(0.413295909766549,-10.4664423611608,
-0.617661468019164));
#31103=CARTESIAN_POINT('Ctrl Pts',(0.472544472511383,-8.90922609310004,
-5.52753257240065));
#31104=CARTESIAN_POINT('Ctrl Pts',(0.531793035256219,-5.20171515149495,
-9.10330010082978));
#31105=CARTESIAN_POINT('Ctrl Pts',(0.591041598001052,-0.23874007198555,
-10.4819341046316));
#31106=CARTESIAN_POINT('Ctrl Pts',(0.650290160745889,4.78185742115312,-9.33068794050316));
#31107=CARTESIAN_POINT('Ctrl Pts',(0.709538723490722,8.64832326230869,-5.92743167035388));
#31108=CARTESIAN_POINT('Ctrl Pts',(0.768787286235557,10.4274692096169,-1.09354201610874));
#31109=CARTESIAN_POINT('Ctrl Pts',(0.828035848980392,9.68987600895932,4.00425592589309));
#31110=CARTESIAN_POINT('Ctrl Pts',(0.887284411725228,6.61358904227201,8.1356504120078));
#31111=CARTESIAN_POINT('Ctrl Pts',(0.946532974470063,1.9410441333556,10.3033660965346));
#31112=CARTESIAN_POINT('Ctrl Pts',(1.0057815372149,-3.19992697648555,9.98448014714238));
#31113=CARTESIAN_POINT('Ctrl Pts',(1.06503009995973,-7.56868573973501,7.25543921015781));
#31114=CARTESIAN_POINT('Ctrl Pts',(1.12427866270457,-10.1104842470233,2.77592039631992));
#31115=CARTESIAN_POINT('Ctrl Pts',(1.1835272254494,-10.2124968952733,-2.37492141025147));
#31116=CARTESIAN_POINT('Ctrl Pts',(1.22302626727929,-8.63654184006421,-5.42462430472119));
#31117=CARTESIAN_POINT('Ctrl Pts',(1.24277578819424,-7.53281147710298,-6.67095206495486));
#31118=CARTESIAN_POINT('Ctrl Pts',(-8.08092526273141,-2.56718148514231,
9.58401523906448));
#31119=CARTESIAN_POINT('Ctrl Pts',(-8.06117574181647,-4.15288747065075,
9.15926684861076));
#31120=CARTESIAN_POINT('Ctrl Pts',(-8.02167669998656,-7.10788292477239,
7.50811752606706));
#31121=CARTESIAN_POINT('Ctrl Pts',(-7.96242813724176,-9.82562146195453,
3.21612905681762));
#31122=CARTESIAN_POINT('Ctrl Pts',(-7.9031795744969,-10.1715216087662,-1.85075158985345));
#31123=CARTESIAN_POINT('Ctrl Pts',(-7.84393101175209,-8.06265137515507,
-6.47160554253427));
#31124=CARTESIAN_POINT('Ctrl Pts',(-7.78468244900723,-4.0077163292958,-9.53015895490345));
#31125=CARTESIAN_POINT('Ctrl Pts',(-7.72543388626241,1.01445492917372,-10.288728093667));
#31126=CARTESIAN_POINT('Ctrl Pts',(-7.66618532351757,5.79180729210547,-8.56396079873138));
#31127=CARTESIAN_POINT('Ctrl Pts',(-7.60693676077273,9.17125936598514,-4.77227811905034));
#31128=CARTESIAN_POINT('Ctrl Pts',(-7.54768819802789,10.3371806995511,0.171246530947913));
#31129=CARTESIAN_POINT('Ctrl Pts',(-7.48843963528308,9.00815878071438,5.07342716128625));
#31130=CARTESIAN_POINT('Ctrl Pts',(-7.42919107253822,5.50496634762878,8.75111271197646));
#31131=CARTESIAN_POINT('Ctrl Pts',(-7.3699425097934,0.673116783527759,10.3166620838708));
#31132=CARTESIAN_POINT('Ctrl Pts',(-7.31069394704856,-4.32119299704472,
9.39222583643303));
#31133=CARTESIAN_POINT('Ctrl Pts',(-7.25144538430372,-8.27255756220144,
6.20091945257043));
#31134=CARTESIAN_POINT('Ctrl Pts',(-7.19219682155889,-10.2272913249547,
1.51298497558452));
#31135=CARTESIAN_POINT('Ctrl Pts',(-7.13294825881406,-9.71360793964782,
-3.54011761331254));
#31136=CARTESIAN_POINT('Ctrl Pts',(-7.07369969606921,-6.85548782274077,
-7.73879176313041));
#31137=CARTESIAN_POINT('Ctrl Pts',(-7.0144511333244,-2.34275521392854,-10.0696628406093));
#31138=CARTESIAN_POINT('Ctrl Pts',(-6.95520257057954,2.73541522398385,-9.9701612333058));
#31139=CARTESIAN_POINT('Ctrl Pts',(-6.89595400783472,7.15337702289769,-7.46430229388277));
#31140=CARTESIAN_POINT('Ctrl Pts',(-6.83670544508987,9.84482899455965,-3.15688986340601));
#31141=CARTESIAN_POINT('Ctrl Pts',(-6.77745688234505,10.1601732918617,1.91245659202953));
#31142=CARTESIAN_POINT('Ctrl Pts',(-6.71820831960021,8.02329970660245,6.5202203464263));
#31143=CARTESIAN_POINT('Ctrl Pts',(-6.65895975685538,3.94995530911404,9.55429037633348));
#31144=CARTESIAN_POINT('Ctrl Pts',(-6.59971119411054,-1.07673415119273,
10.2823759468273));
#31145=CARTESIAN_POINT('Ctrl Pts',(-6.54046263136571,-5.84354745936712,
8.52874930058177));
#31146=CARTESIAN_POINT('Ctrl Pts',(-6.48121406862087,-9.19998604553876,
4.71665859529904));
#31147=CARTESIAN_POINT('Ctrl Pts',(-6.42196550587603,-10.3359536162835,
-0.233825543369873));
#31148=CARTESIAN_POINT('Ctrl Pts',(-6.36271694313121,-8.97727768338141,
-5.12787450489945));
#31149=CARTESIAN_POINT('Ctrl Pts',(-6.30346838038635,-5.45188271472368,
-8.78428064257877));
#31150=CARTESIAN_POINT('Ctrl Pts',(-6.24421981764154,-0.610643625455016,
-10.3205487211332));
#31151=CARTESIAN_POINT('Ctrl Pts',(-6.18497125489669,4.37797791247879,-9.3658913585673));
#31152=CARTESIAN_POINT('Ctrl Pts',(-6.12572269215187,8.30994860194132,-6.15072075253911));
#31153=CARTESIAN_POINT('Ctrl Pts',(-6.06647412940703,10.2362640741913,-1.45103733447644));
#31154=CARTESIAN_POINT('Ctrl Pts',(-6.00722556666219,9.69199670308129,3.59886252169872));
#31155=CARTESIAN_POINT('Ctrl Pts',(-5.94797700391735,6.80850863592549,7.78015563450705));
#31156=CARTESIAN_POINT('Ctrl Pts',(-5.88872844117253,2.28174676273358,10.0836621945293));
#31157=CARTESIAN_POINT('Ctrl Pts',(-5.82947987842768,-2.79572817960588,
9.9534172769146));
#31158=CARTESIAN_POINT('Ctrl Pts',(-5.77023131568286,-7.19843759956617,
7.42085626243881));
#31159=CARTESIAN_POINT('Ctrl Pts',(-5.71098275293802,-9.86376155315033,
3.09722772253158));
#31160=CARTESIAN_POINT('Ctrl Pts',(-5.65173419019319,-10.1484083487808,
-1.97393503667728));
#31161=CARTESIAN_POINT('Ctrl Pts',(-5.59248562744834,-7.98367679971535,
-6.56867690637251));
#31162=CARTESIAN_POINT('Ctrl Pts',(-5.53323706470353,-3.8920376615774,-9.57802977566305));
#31163=CARTESIAN_POINT('Ctrl Pts',(-5.47398850195867,1.1389677729664,-10.2756685405266));
#31164=CARTESIAN_POINT('Ctrl Pts',(-5.41473993921385,5.89507660278836,-8.49321396115051));
#31165=CARTESIAN_POINT('Ctrl Pts',(-5.35549137646901,9.22837384729142,-4.66087198679098));
#31166=CARTESIAN_POINT('Ctrl Pts',(-5.29624281372418,10.3343485125815,0.29639899313195));
#31167=CARTESIAN_POINT('Ctrl Pts',(-5.23699425097934,8.9460670755048,5.18213232397573));
#31168=CARTESIAN_POINT('Ctrl Pts',(-5.1777456882345,5.39859946737001,8.81712738557956));
#31169=CARTESIAN_POINT('Ctrl Pts',(-5.11849712548967,0.548147965346974,
10.3240566324828));
#31170=CARTESIAN_POINT('Ctrl Pts',(-5.05924856274483,-4.43460228834889,
9.33921378311876));
#31171=CARTESIAN_POINT('Ctrl Pts',(-5.,-8.34703506573574,6.10029648082801));
#31172=CARTESIAN_POINT('Ctrl Pts',(-4.94075143725517,-10.2448615886467,
1.38903656254868));
#31173=CARTESIAN_POINT('Ctrl Pts',(-4.88150287451033,-9.67003020726149,
-3.65747554103578));
#31174=CARTESIAN_POINT('Ctrl Pts',(-4.8222543117655,-6.76127987344612,-7.82123430256102));
#31175=CARTESIAN_POINT('Ctrl Pts',(-4.76300574902066,-2.22065467459968,
-10.0972919319392));
#31176=CARTESIAN_POINT('Ctrl Pts',(-4.70375718627583,2.85593865679291,-9.93630846598779));
#31177=CARTESIAN_POINT('Ctrl Pts',(-4.64450862353099,7.24323431121841,-7.37713821582688));
#31178=CARTESIAN_POINT('Ctrl Pts',(-4.58526006078616,9.88233254810626,-3.03745204921238));
#31179=CARTESIAN_POINT('Ctrl Pts',(-4.52601149804132,10.1362714076301,2.03534112459961));
#31180=CARTESIAN_POINT('Ctrl Pts',(-4.46676293529649,7.94376124494917,6.61689268659152));
#31181=CARTESIAN_POINT('Ctrl Pts',(-4.40751437255165,3.83397734828913,9.60141808460764));
#31182=CARTESIAN_POINT('Ctrl Pts',(-4.34826580980682,-1.20115964495595,
10.268584471579));
#31183=CARTESIAN_POINT('Ctrl Pts',(-4.28901724706198,-5.94638965754321,
8.45736729622688));
#31184=CARTESIAN_POINT('Ctrl Pts',(-4.22976868431715,-9.25642337572245,
4.60491453036902));
#31185=CARTESIAN_POINT('Ctrl Pts',(-4.17052012157231,-10.3323645951943,
-0.358961578166624));
#31186=CARTESIAN_POINT('Ctrl Pts',(-4.11127155882748,-8.91452854248819,
-5.23620018790229));
#31187=CARTESIAN_POINT('Ctrl Pts',(-4.05202299608264,-5.34511833009956,
-8.849650929831));
#31188=CARTESIAN_POINT('Ctrl Pts',(-3.99277443333781,-0.485632212442896,
-10.3271861073994));
#31189=CARTESIAN_POINT('Ctrl Pts',(-3.93352587059297,4.49106411037733,-9.31219387143038));
#31190=CARTESIAN_POINT('Ctrl Pts',(-3.87427730784814,8.38381556238237,-6.04964859794188));
#31191=CARTESIAN_POINT('Ctrl Pts',(-3.8150287451033,10.2530835696273,-1.32698487439137));
#31192=CARTESIAN_POINT('Ctrl Pts',(-3.75578018235847,9.64770924886438,3.71595449272479));
#31193=CARTESIAN_POINT('Ctrl Pts',(-3.69653161961364,6.713803270925,7.86202627710832));
#31194=CARTESIAN_POINT('Ctrl Pts',(-3.6372830568688,2.15948118661882,10.1105515451564));
#31195=CARTESIAN_POINT('Ctrl Pts',(-3.57803449412396,-2.91604444729796,
9.91883543184418));
#31196=CARTESIAN_POINT('Ctrl Pts',(-3.51878593137913,-7.2877655164092,7.33314975440033));
#31197=CARTESIAN_POINT('Ctrl Pts',(-3.45953736863429,-9.90054129837521,
2.97756503569476));
#31198=CARTESIAN_POINT('Ctrl Pts',(-3.40028880588946,-10.1237629134634,
-2.09667260548911));
#31199=CARTESIAN_POINT('Ctrl Pts',(-3.34104024314462,-7.90355450535475,
-6.66486591939489));
#31200=CARTESIAN_POINT('Ctrl Pts',(-3.28179168039979,-3.77577649753992,
-9.62445444600628));
#31201=CARTESIAN_POINT('Ctrl Pts',(-3.22254311765495,1.26330748749216,-10.2611239995758));
#31202=CARTESIAN_POINT('Ctrl Pts',(-3.16329455491012,5.99748474269926,-8.42121061984051));
#31203=CARTESIAN_POINT('Ctrl Pts',(-3.10404599216528,9.28413360266045,-4.54878827717624));
#31204=CARTESIAN_POINT('Ctrl Pts',(-3.04479742942045,10.3300019368408,0.421511005181756));
#31205=CARTESIAN_POINT('Ctrl Pts',(-2.98554886667561,8.88266324040311,5.29007611478477));
#31206=CARTESIAN_POINT('Ctrl Pts',(-2.92630030393078,5.29144126330465,8.88185008315394));
#31207=CARTESIAN_POINT('Ctrl Pts',(-2.86705174118594,0.423098658307396,
10.3299370311713));
#31208=CARTESIAN_POINT('Ctrl Pts',(-2.80780317844112,-4.54736130891176,
9.28483261393749));
#31209=CARTESIAN_POINT('Ctrl Pts',(-2.74855461569627,-8.42028874366297,
5.99877896041916));
#31210=CARTESIAN_POINT('Ctrl Pts',(-2.68930605295144,-10.2609297157501,
1.26488454455777));
#31211=CARTESIAN_POINT('Ctrl Pts',(-2.63005749020661,-9.62503464608216,
-3.77429723317373));
#31212=CARTESIAN_POINT('Ctrl Pts',(-2.57080892746177,-6.66608056865438,
-7.90253006288704));
#31213=CARTESIAN_POINT('Ctrl Pts',(-2.51156036471693,-2.09822854115333,
-10.1234405481395));
#31214=CARTESIAN_POINT('Ctrl Pts',(-2.4523118019721,2.97604334789586,-9.90099881497165));
#31215=CARTESIAN_POINT('Ctrl Pts',(-2.39306323922727,7.33202958281215,-7.2888924905909));
#31216=CARTESIAN_POINT('Ctrl Pts',(-2.33381467648243,9.91838713650106,-2.91756887718436));
#31217=CARTESIAN_POINT('Ctrl Pts',(-2.2745661137376,10.1108833247894,2.15792723119204));
#31218=CARTESIAN_POINT('Ctrl Pts',(-2.21531755099276,7.86305805474182,6.71259484628595));
#31219=CARTESIAN_POINT('Ctrl Pts',(-2.15606898824793,3.71743724272782,9.64713801544299));
#31220=CARTESIAN_POINT('Ctrl Pts',(-2.09682042550309,-1.325409022497,10.2532873979865));
#31221=CARTESIAN_POINT('Ctrl Pts',(-2.03757186275826,-6.04835998532599,
8.38474525734275));
#31222=CARTESIAN_POINT('Ctrl Pts',(-1.97832330001343,-9.31150351236521,
4.49249528456464));
#31223=CARTESIAN_POINT('Ctrl Pts',(-1.91907473726858,-10.3272606241262,
-0.484044981378821));
#31224=CARTESIAN_POINT('Ctrl Pts',(-1.85982617452376,-8.85047233729729,
-5.34375812975856));
#31225=CARTESIAN_POINT('Ctrl Pts',(-1.80057761177891,-5.23757023456047,
-8.9137236652631));
#31226=CARTESIAN_POINT('Ctrl Pts',(-1.74132904903408,-0.360549595157115,
-10.3323093029611));
#31227=CARTESIAN_POINT('Ctrl Pts',(-1.68208048628925,4.60349182033403,-9.25713101358854));
#31228=CARTESIAN_POINT('Ctrl Pts',(-1.62283192354441,8.45645327262435,-5.94768943292654));
#31229=CARTESIAN_POINT('Ctrl Pts',(-1.56358336079958,10.2683997394084,-1.20273784938449));
#31230=CARTESIAN_POINT('Ctrl Pts',(-1.50433479805474,9.60200723007033,3.83250162378335));
#31231=CARTESIAN_POINT('Ctrl Pts',(-1.44508623530991,6.61811351594752,7.94274417519902));
#31232=CARTESIAN_POINT('Ctrl Pts',(-1.38583767256507,2.0368989834672,10.1359584684318));
#31233=CARTESIAN_POINT('Ctrl Pts',(-1.32658910982024,-3.03593315927972,
9.88279926918536));
#31234=CARTESIAN_POINT('Ctrl Pts',(-1.26734054707541,-7.37602488789294,
7.2443680466835));
#31235=CARTESIAN_POINT('Ctrl Pts',(-1.20809198433057,-9.93586940833061,
2.8574657728877));
#31236=CARTESIAN_POINT('Ctrl Pts',(-1.14884342158574,-10.0976331137197,
-2.21910275637184));
#31237=CARTESIAN_POINT('Ctrl Pts',(-1.0895948588409,-7.8222733775397,-6.76007771772325));
#31238=CARTESIAN_POINT('Ctrl Pts',(-1.03034629609607,-3.65896172232424,
-9.66946796143364));
#31239=CARTESIAN_POINT('Ctrl Pts',(-0.971097733351229,1.38746197358963,
-10.2450749540678));
#31240=CARTESIAN_POINT('Ctrl Pts',(-0.911849170606397,6.09901352055129,
-8.34797254540039));
#31241=CARTESIAN_POINT('Ctrl Pts',(-0.852600607861559,9.33853210157117,
-4.43603761599793));
#31242=CARTESIAN_POINT('Ctrl Pts',(-0.793352045116727,10.3241407575351,
0.546561214525285));
#31243=CARTESIAN_POINT('Ctrl Pts',(-0.734103482371892,8.81795701315387,
5.39724426506792));
#31244=CARTESIAN_POINT('Ctrl Pts',(-0.674854919627056,5.18350721855164,
8.94527050780554));
#31245=CARTESIAN_POINT('Ctrl Pts',(-0.615606356882222,0.297987315778273,
10.3343028358144));
#31246=CARTESIAN_POINT('Ctrl Pts',(-0.556357794137386,-4.65945358713783,
9.22909008580174));
#31247=CARTESIAN_POINT('Ctrl Pts',(-0.497109231392552,-8.49230782362366,
5.89638188820198));
#31248=CARTESIAN_POINT('Ctrl Pts',(-0.437860668647716,-10.2754933667894,
1.14054706688608));
#31249=CARTESIAN_POINT('Ctrl Pts',(-0.378612105902882,-9.57862784490375,
-3.89056553098446));
#31250=CARTESIAN_POINT('Ctrl Pts',(-0.319363543158048,-6.56990387110002,
-7.98266714004419));
#31251=CARTESIAN_POINT('Ctrl Pts',(-0.260114980413213,-1.97549476159458,
-10.1481048470248));
#31252=CARTESIAN_POINT('Ctrl Pts',(-0.200866417668376,3.09571168604639,
-9.86423746190218));
#31253=CARTESIAN_POINT('Ctrl Pts',(-0.141617854923542,7.4197498191524,-7.19957805418105));
#31254=CARTESIAN_POINT('Ctrl Pts',(-0.0823692921787063,9.95298747268358,
-2.79725792704241));
#31255=CARTESIAN_POINT('Ctrl Pts',(-0.0231207294338726,10.0840127666341,
2.28019694073663));
#31256=CARTESIAN_POINT('Ctrl Pts',(0.036127833310962,7.78120196742404,6.80731278904333));
#31257=CARTESIAN_POINT('Ctrl Pts',(0.0953763960557959,3.60035208234145,
9.69144347345206));
#31258=CARTESIAN_POINT('Ctrl Pts',(0.154624958800632,-1.44946407108565,
10.2364869534169));
#31259=CARTESIAN_POINT('Ctrl Pts',(0.213873521545467,-6.14944348214002,
8.31089386174798));
#31260=CARTESIAN_POINT('Ctrl Pts',(0.273122084290302,-9.36521839784525,
4.37941728344064));
#31261=CARTESIAN_POINT('Ctrl Pts',(0.332370647035137,-10.3206424160579,
-0.609057301959502));
#31262=CARTESIAN_POINT('Ctrl Pts',(0.391619209779971,-8.78511852813569,
-5.45053277458957));
#31263=CARTESIAN_POINT('Ctrl Pts',(0.450867772524806,-5.1292540651622,-8.97648904037991));
#31264=CARTESIAN_POINT('Ctrl Pts',(0.510116335269641,-0.235414367969966,
-10.3359183559853));
#31265=CARTESIAN_POINT('Ctrl Pts',(0.569364898014477,4.71524504940002,-9.20070931524018));
#31266=CARTESIAN_POINT('Ctrl Pts',(0.628613460759311,8.52785013367849,-5.84486118629469));
#31267=CARTESIAN_POINT('Ctrl Pts',(0.687862023504145,10.2822121694629,-1.07830872475579));
#31268=CARTESIAN_POINT('Ctrl Pts',(0.74711058624898,9.55489381143604,3.94847572150008));
#31269=CARTESIAN_POINT('Ctrl Pts',(0.806359148993816,6.52146022848571,8.02231893388788));
#31270=CARTESIAN_POINT('Ctrl Pts',(0.865607711738651,1.91400494292965,10.159837841239));
#31271=CARTESIAN_POINT('Ctrl Pts',(0.924856274483484,-3.15535125902531,
9.84539404633543));
#31272=CARTESIAN_POINT('Ctrl Pts',(0.98410483722832,-7.46325220967044,7.15436927616918));
#31273=CARTESIAN_POINT('Ctrl Pts',(1.04335339997316,-9.96964288017544,2.73725118786993));
#31274=CARTESIAN_POINT('Ctrl Pts',(1.10260196271799,-10.0702344688141,-2.34183820974359));
#31275=CARTESIAN_POINT('Ctrl Pts',(1.14210100454788,-8.51623282935078,-5.34905804270582));
#31276=CARTESIAN_POINT('Ctrl Pts',(1.16185052546282,-7.42787768375332,-6.5780241710925));
#31277=CARTESIAN_POINT('Ctrl Pts',(-8.16185052546282,-2.53091485516775,
9.44862164248498));
#31278=CARTESIAN_POINT('Ctrl Pts',(-8.14210100454788,-4.09421953692821,
9.02987368199619));
#31279=CARTESIAN_POINT('Ctrl Pts',(-8.10260196271799,-7.00746970450451,
7.40205018267925));
#31280=CARTESIAN_POINT('Ctrl Pts',(-8.04335339997316,-9.68681468888719,
3.17069473005534));
#31281=CARTESIAN_POINT('Ctrl Pts',(-7.98410483722832,-10.0278282966267,
-1.82460598095417));
#31282=CARTESIAN_POINT('Ctrl Pts',(-7.92485627448349,-7.94875011973976,
-6.38018102700592));
#31283=CARTESIAN_POINT('Ctrl Pts',(-7.86560771173864,-3.95109923151803,
-9.3955261872489));
#31284=CARTESIAN_POINT('Ctrl Pts',(-7.80635914899382,1.00012370181206,-10.1433790029068));
#31285=CARTESIAN_POINT('Ctrl Pts',(-7.74711058624898,5.70998630159022,-8.44297753393233));
#31286=CARTESIAN_POINT('Ctrl Pts',(-7.68786202350414,9.04169678081072,-4.70486003985297));
#31287=CARTESIAN_POINT('Ctrl Pts',(-7.62861346075931,10.1911471177493,0.168827327394019));
#31288=CARTESIAN_POINT('Ctrl Pts',(-7.56936489801448,8.88090032113799,5.00175474286701));
#31289=CARTESIAN_POINT('Ctrl Pts',(-7.51011633526964,5.42719756551993,8.6274855479338));
#31290=CARTESIAN_POINT('Ctrl Pts',(-7.45086777252481,0.663607647746304,
10.1709183690093));
#31291=CARTESIAN_POINT('Ctrl Pts',(-7.39161920977997,-4.26014740740508,
9.25954165301287));
#31292=CARTESIAN_POINT('Ctrl Pts',(-7.33237064703514,-8.15569095741015,
6.11331892545928));
#31293=CARTESIAN_POINT('Ctrl Pts',(-7.27312208429031,-10.0828101527934,
1.49161100316218));
#31294=CARTESIAN_POINT('Ctrl Pts',(-7.21387352154547,-9.57638358410301,
-3.49010629300211));
#31295=CARTESIAN_POINT('Ctrl Pts',(-7.15462495880062,-6.75864019369647,
-7.62946567966184));
#31296=CARTESIAN_POINT('Ctrl Pts',(-7.0953763960558,-2.30965905888213,-9.92740848955444));
#31297=CARTESIAN_POINT('Ctrl Pts',(-7.03612783331096,2.69677195223654,-9.82931254367178));
#31298=CARTESIAN_POINT('Ctrl Pts',(-6.97687927056613,7.0523211064931,-7.35885392925516));
#31299=CARTESIAN_POINT('Ctrl Pts',(-6.91763070782129,9.70575087625173,-3.11229241004746));
#31300=CARTESIAN_POINT('Ctrl Pts',(-6.85838214507646,10.0166402976476,1.88543927519122));
#31301=CARTESIAN_POINT('Ctrl Pts',(-6.79913358233163,7.90995437308458,6.42810904848144));
#31302=CARTESIAN_POINT('Ctrl Pts',(-6.73988501958678,3.89415420255387,9.41931670355132));
#31303=CARTESIAN_POINT('Ctrl Pts',(-6.68063645684196,-1.06152310387555,
10.1371165929868));
#31304=CARTESIAN_POINT('Ctrl Pts',(-6.62138789409712,-5.76099553435745,
8.4082634694007));
#31305=CARTESIAN_POINT('Ctrl Pts',(-6.56213933135228,-9.07001763792296,
4.65002625435157));
#31306=CARTESIAN_POINT('Ctrl Pts',(-6.50289076860745,-10.1899373695142,
-0.230522284714781));
#31307=CARTESIAN_POINT('Ctrl Pts',(-6.44364220586261,-8.85045548175431,
-5.05543290764522));
#31308=CARTESIAN_POINT('Ctrl Pts',(-6.38439364311778,-5.3748638462783,-8.66018491444234));
#31309=CARTESIAN_POINT('Ctrl Pts',(-6.32514508037295,-0.602017049368022,
-10.1747500996605));
#31310=CARTESIAN_POINT('Ctrl Pts',(-6.26589651762811,4.31613012107503,-9.23357920290205));
#31311=CARTESIAN_POINT('Ctrl Pts',(-6.20664795488327,8.19255377309947,-6.06382938358051));
#31312=CARTESIAN_POINT('Ctrl Pts',(-6.14739939213844,10.0916561438018,-1.4305384977587));
#31313=CARTESIAN_POINT('Ctrl Pts',(-6.0881508293936,9.55507764995644,3.54802131076013));
#31314=CARTESIAN_POINT('Ctrl Pts',(-6.02890226664877,6.71232468289887,7.67024520270696));
#31315=CARTESIAN_POINT('Ctrl Pts',(-5.96965370390394,2.24951247543498,9.9412100742901));
#31316=CARTESIAN_POINT('Ctrl Pts',(-5.91040514115909,-2.75623286539221,
9.81280512952515));
#31317=CARTESIAN_POINT('Ctrl Pts',(-5.85115657841427,-7.09674511139212,
7.31602166086433));
#31318=CARTESIAN_POINT('Ctrl Pts',(-5.79190801566943,-9.72441597416585,
3.05347311756495));
#31319=CARTESIAN_POINT('Ctrl Pts',(-5.7326594529246,-10.0050415581794,-1.94604921248318));
#31320=CARTESIAN_POINT('Ctrl Pts',(-5.67341089017976,-7.87089121988491,
-6.47588106152688));
#31321=CARTESIAN_POINT('Ctrl Pts',(-5.61416232743493,-3.83705475891298,
-9.44272073585823));
#31322=CARTESIAN_POINT('Ctrl Pts',(-5.55491376469009,1.12287754988938,-10.1305039423643));
#31323=CARTESIAN_POINT('Ctrl Pts',(-5.49566520194526,5.81179672442278,-8.37323013850045));
#31324=CARTESIAN_POINT('Ctrl Pts',(-5.43641663920042,9.09800440456847,-4.59502774450345));
#31325=CARTESIAN_POINT('Ctrl Pts',(-5.37716807645559,10.188354941148,0.292211757959466));
#31326=CARTESIAN_POINT('Ctrl Pts',(-5.31791951371075,8.81968578682977,5.10892422530387));
#31327=CARTESIAN_POINT('Ctrl Pts',(-5.25867095096592,5.32233333254584,8.69256763077374));
#31328=CARTESIAN_POINT('Ctrl Pts',(-5.19942238822108,0.5404042668412,10.1782084546684));
#31329=CARTESIAN_POINT('Ctrl Pts',(-5.14017382547625,-4.37195456312701,
9.2072785021556));
#31330=CARTESIAN_POINT('Ctrl Pts',(-5.08092526273141,-8.2291163155945,6.01411745667809));
#31331=CARTESIAN_POINT('Ctrl Pts',(-5.02167669998658,-10.1001322009791,
1.36941361211582));
#31332=CARTESIAN_POINT('Ctrl Pts',(-4.96242813724175,-9.53342147531196,
-3.60580630266854));
#31333=CARTESIAN_POINT('Ctrl Pts',(-4.9031795744969,-6.66576312219815,-7.71074355150312));
#31334=CARTESIAN_POINT('Ctrl Pts',(-4.84393101175208,-2.18928343658979,
-9.95464726409617));
#31335=CARTESIAN_POINT('Ctrl Pts',(-4.78468244900724,2.815592747828,-9.79593801515108));
#31336=CARTESIAN_POINT('Ctrl Pts',(-4.72543388626241,7.14090897890188,-7.27292122006985));
#31337=CARTESIAN_POINT('Ctrl Pts',(-4.66618532351757,9.74272461626274,-2.99454189651309));
#31338=CARTESIAN_POINT('Ctrl Pts',(-4.60693676077273,9.99307607586648,2.00658781523482));
#31339=CARTESIAN_POINT('Ctrl Pts',(-4.5476881980279,7.83153955304924,6.52341569634566));
#31340=CARTESIAN_POINT('Ctrl Pts',(-4.48843963528306,3.7798146649627,9.46577863764184));
#31341=CARTESIAN_POINT('Ctrl Pts',(-4.42919107253823,-1.18419083591923,
10.1235199502164));
#31342=CARTESIAN_POINT('Ctrl Pts',(-4.36994250979339,-5.8623848785111,8.33788988020998));
#31343=CARTESIAN_POINT('Ctrl Pts',(-4.31069394704856,-9.12565767668712,
4.53986080031373));
#31344=CARTESIAN_POINT('Ctrl Pts',(-4.25144538430373,-10.1863990506059,
-0.353890519962989));
#31345=CARTESIAN_POINT('Ctrl Pts',(-4.19219682155889,-8.78859279937101,
-5.16222827131344));
#31346=CARTESIAN_POINT('Ctrl Pts',(-4.13294825881405,-5.26960772449185,
-8.7246317141917));
#31347=CARTESIAN_POINT('Ctrl Pts',(-4.07369969606922,-0.478771675369725,
-10.1812937194233));
#31348=CARTESIAN_POINT('Ctrl Pts',(-4.01445113332438,4.42761874773907,-9.18064030136098));
#31349=CARTESIAN_POINT('Ctrl Pts',(-3.95520257057955,8.26537721334642,-5.96418507756067));
#31350=CARTESIAN_POINT('Ctrl Pts',(-3.89595400783471,10.1082380298515,-1.30823852953812));
#31351=CARTESIAN_POINT('Ctrl Pts',(-3.83670544508988,9.51141584559089,3.66345912090558));
#31352=CARTESIAN_POINT('Ctrl Pts',(-3.77745688234504,6.61895722269747,7.75095925691813));
#31353=CARTESIAN_POINT('Ctrl Pts',(-3.71820831960021,2.12897414783507,9.96771955846239));
#31354=CARTESIAN_POINT('Ctrl Pts',(-3.65895975685538,-2.8748494224929,9.7787118229497));
#31355=CARTESIAN_POINT('Ctrl Pts',(-3.59971119411054,-7.18481109076589,
7.22955418461685));
#31356=CARTESIAN_POINT('Ctrl Pts',(-3.5404626313657,-9.76067613111137,2.93550090816825));
#31357=CARTESIAN_POINT('Ctrl Pts',(-3.48121406862087,-9.98074428947528,
-2.06705286492883));
#31358=CARTESIAN_POINT('Ctrl Pts',(-3.42196550587603,-7.7919008149599,-6.57071121022154));
#31359=CARTESIAN_POINT('Ctrl Pts',(-3.3627169431312,-3.72243601892731,-9.48848956385033));
#31360=CARTESIAN_POINT('Ctrl Pts',(-3.30346838038636,1.2454607145008,-10.1161648724672));
#31361=CARTESIAN_POINT('Ctrl Pts',(-3.24421981764153,5.91275814226201,-8.3022439899956));
#31362=CARTESIAN_POINT('Ctrl Pts',(-3.1849712548967,9.15297644063244,-4.48452744394893));
#31363=CARTESIAN_POINT('Ctrl Pts',(-3.12572269215187,10.1840697695796,0.415556309830607));
#31364=CARTESIAN_POINT('Ctrl Pts',(-3.06647412940702,8.75717765911764,5.21534309177781));
#31365=CARTESIAN_POINT('Ctrl Pts',(-3.0072255666622,5.21668895481417,8.75637598935904));
#31366=CARTESIAN_POINT('Ctrl Pts',(-2.94797700391735,0.417121534145209,
10.1840057808338));
#31367=CARTESIAN_POINT('Ctrl Pts',(-2.88872844117253,-4.48312063449688,
9.15366557696162));
#31368=CARTESIAN_POINT('Ctrl Pts',(-2.82947987842769,-8.30133513718334,
5.91403407653938));
#31369=CARTESIAN_POINT('Ctrl Pts',(-2.77023131568285,-10.1159733332934,
1.24701549244614));
#31370=CARTESIAN_POINT('Ctrl Pts',(-2.71098275293802,-9.4890615674268,-3.72097765216174));
#31371=CARTESIAN_POINT('Ctrl Pts',(-2.65173419019319,-6.57190870010391,
-7.79089084481372));
#31372=CARTESIAN_POINT('Ctrl Pts',(-2.59248562744835,-2.0685868198553,-9.98042647821348));
#31373=CARTESIAN_POINT('Ctrl Pts',(-2.53323706470351,2.93400071728676,-9.76112718436066));
#31374=CARTESIAN_POINT('Ctrl Pts',(-2.47398850195868,7.22844983771763,-7.18592214415825));
#31375=CARTESIAN_POINT('Ctrl Pts',(-2.41473993921385,9.77826986068487,-2.87635231672436));
#31376=CARTESIAN_POINT('Ctrl Pts',(-2.35549137646901,9.96804665103716,2.1274421451712));
#31377=CARTESIAN_POINT('Ctrl Pts',(-2.29624281372417,7.75197645860605,6.61776586950019));
#31378=CARTESIAN_POINT('Ctrl Pts',(-2.23699425097934,3.6649209240663,9.51085268199676));
#31379=CARTESIAN_POINT('Ctrl Pts',(-2.1777456882345,-1.30668493973852,10.1084389787229));
#31380=CARTESIAN_POINT('Ctrl Pts',(-2.11849712548967,-5.96291466920391,
8.26629377448541));
#31381=CARTESIAN_POINT('Ctrl Pts',(-2.05924856274484,-9.17995969501367,
4.42902970369678));
#31382=CARTESIAN_POINT('Ctrl Pts',(-2.,-10.1813671834506,-0.477206867154204));
#31383=CARTESIAN_POINT('Ctrl Pts',(-1.94075143725517,-8.72544151761641,
-5.26826673973136));
#31384=CARTESIAN_POINT('Ctrl Pts',(-1.88150287451033,-5.163578963292,-8.78779929266436));
#31385=CARTESIAN_POINT('Ctrl Pts',(-1.8222543117655,-0.355456103002113,
-10.1863445394873));
#31386=CARTESIAN_POINT('Ctrl Pts',(-1.76300574902066,4.53845818893508,-9.1263553177373));
#31387=CARTESIAN_POINT('Ctrl Pts',(-1.70375718627583,8.33698876903922,-5.86366629193867));
#31388=CARTESIAN_POINT('Ctrl Pts',(-1.64450862353099,10.1233378277612,-1.18574674501868));
#31389=CARTESIAN_POINT('Ctrl Pts',(-1.58526006078616,9.46635946023347,3.77835978804986));
#31390=CARTESIAN_POINT('Ctrl Pts',(-1.52601149804132,6.52461927901817,7.83053685146607));
#31391=CARTESIAN_POINT('Ctrl Pts',(-1.46676293529649,2.00812366619552,9.99276755756728));
#31392=CARTESIAN_POINT('Ctrl Pts',(-1.40751437255165,-2.99304446397231,
9.74318474396275));
#31393=CARTESIAN_POINT('Ctrl Pts',(-1.34826580980682,-7.27182362014442,
7.14202669806083));
#31394=CARTESIAN_POINT('Ctrl Pts',(-1.28901724706198,-9.7955051600712,2.81709829031974));
#31395=CARTESIAN_POINT('Ctrl Pts',(-1.22976868431715,-9.95498362599407,
-2.1877534423453));
#31396=CARTESIAN_POINT('Ctrl Pts',(-1.17052012157231,-7.71176794744644,
-6.66457794935592));
#31397=CARTESIAN_POINT('Ctrl Pts',(-1.11127155882748,-3.60727148864087,
-9.53286717234345));
#31398=CARTESIAN_POINT('Ctrl Pts',(-1.05202299608264,1.36786126741004,-10.1003425521822));
#31399=CARTESIAN_POINT('Ctrl Pts',(-0.992774433337809,6.01285262080975,
-8.23004055146306));
#31400=CARTESIAN_POINT('Ctrl Pts',(-0.933525870592972,9.20660645073839,
-4.3733696138704));
#31401=CARTESIAN_POINT('Ctrl Pts',(-0.874277307848139,10.1782913912843,
0.538839932083674));
#31402=CARTESIAN_POINT('Ctrl Pts',(-0.815028745103303,8.69338553818084,
5.32099727521684));
#31403=CARTESIAN_POINT('Ctrl Pts',(-0.755780182358468,5.11027969671351,
8.81890047226012));
#31404=CARTESIAN_POINT('Ctrl Pts',(-0.696531619613633,0.293777642336413,
10.1883099096576));
#31405=CARTESIAN_POINT('Ctrl Pts',(-0.637283056868798,-4.59362938261378,
9.09871052476142));
#31406=CARTESIAN_POINT('Ctrl Pts',(-0.578034494123964,-8.37233680199861,
5.81308357004031));
#31407=CARTESIAN_POINT('Ctrl Pts',(-0.518785931379129,-10.1303312433104,
1.12443453308871));
#31408=CARTESIAN_POINT('Ctrl Pts',(-0.459537368634294,-9.44331035616146,
-3.83560342514168));
#31409=CARTESIAN_POINT('Ctrl Pts',(-0.40028880588946,-6.47709069289636,
-7.86989582369838));
#31410=CARTESIAN_POINT('Ctrl Pts',(-0.341040243144624,-1.94758690313188,
-10.0047423439996));
#31411=CARTESIAN_POINT('Ctrl Pts',(-0.281791680399788,3.05197849816094,
-9.72488515974416));
#31412=CARTESIAN_POINT('Ctrl Pts',(-0.222543117654954,7.31493084832684,
-7.09786945477928));
#31413=CARTESIAN_POINT('Ctrl Pts',(-0.163294554910118,9.81238139714809,
-2.75774100205266));
#31414=CARTESIAN_POINT('Ctrl Pts',(-0.104045992165285,9.94155569385488,
2.24798454780788));
#31415=CARTESIAN_POINT('Ctrl Pts',(-0.04479742942045,7.67127675405556,6.71114572977224));
#31416=CARTESIAN_POINT('Ctrl Pts',(0.0144511333243838,3.5494898283465,9.5545322358145));
#31417=CARTESIAN_POINT('Ctrl Pts',(0.0736996960692201,-1.42898745989484,
10.0918758744076));
#31418=CARTESIAN_POINT('Ctrl Pts',(0.132948258814054,-6.06257015720878,
8.1934856791998));
#31419=CARTESIAN_POINT('Ctrl Pts',(0.192196821558891,-9.23291574911109,
4.31754915801126));
#31420=CARTESIAN_POINT('Ctrl Pts',(0.251445384303725,-10.174842470955,-0.600453135899833));
#31421=CARTESIAN_POINT('Ctrl Pts',(0.31069394704856,-8.66101096317135,-5.37353297677851));
#31422=CARTESIAN_POINT('Ctrl Pts',(0.369942509793394,-5.05679297882943,
-8.84967797993003));
#31423=CARTESIAN_POINT('Ctrl Pts',(0.429191072538229,-0.232088663954392,
-10.1899026073391));
#31424=CARTESIAN_POINT('Ctrl Pts',(0.488439635283065,4.64863267764692,-9.07073068997722));
#31425=CARTESIAN_POINT('Ctrl Pts',(0.547688198027898,8.40737700504827,-5.76229070223548));
#31426=CARTESIAN_POINT('Ctrl Pts',(0.606936760772733,10.136955129309,-1.06307543340285));
#31427=CARTESIAN_POINT('Ctrl Pts',(0.666185323517568,9.41991161391276,3.89269551710708));
#31428=CARTESIAN_POINT('Ctrl Pts',(0.725433886262404,6.4293314146994,7.90898745576797));
#31429=CARTESIAN_POINT('Ctrl Pts',(0.784682449007238,1.88696575250372,10.0163095859433));
#31430=CARTESIAN_POINT('Ctrl Pts',(0.843931011752074,-3.11077554156509,
9.7063079455285));
#31431=CARTESIAN_POINT('Ctrl Pts',(0.903179574496908,-7.35781867960586,
7.05329934218052));
#31432=CARTESIAN_POINT('Ctrl Pts',(0.962428137241742,-9.82880151332763,
2.69858197941995));
#31433=CARTESIAN_POINT('Ctrl Pts',(1.02167669998658,-9.92797204235483,-2.30875500923572));
#31434=CARTESIAN_POINT('Ctrl Pts',(1.06117574181647,-8.39592381863737,-5.27349178069045));
#31435=CARTESIAN_POINT('Ctrl Pts',(1.08092526273141,-7.32294389040366,-6.48509627723013));
#31436=CARTESIAN_POINT('Ctrl Pts',(-8.24277578819424,-2.49464822519319,
9.31322804590548));
#31437=CARTESIAN_POINT('Ctrl Pts',(-8.22302626727929,-4.03555160320565,
8.90048051538163));
#31438=CARTESIAN_POINT('Ctrl Pts',(-8.1835272254494,-6.90705648423663,7.29598283929145));
#31439=CARTESIAN_POINT('Ctrl Pts',(-8.12427866270457,-9.54800791581985,
3.12526040329305));
#31440=CARTESIAN_POINT('Ctrl Pts',(-8.06503009995973,-9.88413498448718,
-1.79846037205486));
#31441=CARTESIAN_POINT('Ctrl Pts',(-8.0057815372149,-7.83484886432444,-6.28875651147761));
#31442=CARTESIAN_POINT('Ctrl Pts',(-7.94653297447006,-3.89448213374026,
-9.26089341959434));
#31443=CARTESIAN_POINT('Ctrl Pts',(-7.88728441172523,0.985792474450397,
-9.99802991214653));
#31444=CARTESIAN_POINT('Ctrl Pts',(-7.82803584898039,5.62816531107497,-8.32199426913325));
#31445=CARTESIAN_POINT('Ctrl Pts',(-7.76878728623556,8.91213419563631,-4.63744196065562));
#31446=CARTESIAN_POINT('Ctrl Pts',(-7.70953872349072,10.0451135359474,0.166408123840141));
#31447=CARTESIAN_POINT('Ctrl Pts',(-7.65029016074589,8.75364186156157,4.93008232444777));
#31448=CARTESIAN_POINT('Ctrl Pts',(-7.59104159800104,5.3494287834111,8.50385838389115));
#31449=CARTESIAN_POINT('Ctrl Pts',(-7.53179303525623,0.654098511964837,
10.0251746541477));
#31450=CARTESIAN_POINT('Ctrl Pts',(-7.47254447251138,-4.19910181776543,
9.12685746959272));
#31451=CARTESIAN_POINT('Ctrl Pts',(-7.41329590976655,-8.03882435261888,
6.02571839834814));
#31452=CARTESIAN_POINT('Ctrl Pts',(-7.35404734702171,-9.93832898063206,
1.47023703073982));
#31453=CARTESIAN_POINT('Ctrl Pts',(-7.29479878427688,-9.43915922855823,
-3.44009497269169));
#31454=CARTESIAN_POINT('Ctrl Pts',(-7.23555022153204,-6.66179256465216,
-7.52013959619327));
#31455=CARTESIAN_POINT('Ctrl Pts',(-7.17630165878721,-2.27656290383574,
-9.78515413849957));
#31456=CARTESIAN_POINT('Ctrl Pts',(-7.11705309604237,2.65812868048924,-9.68846385403776));
#31457=CARTESIAN_POINT('Ctrl Pts',(-7.05780453329754,6.9512651900885,-7.25340556462755));
#31458=CARTESIAN_POINT('Ctrl Pts',(-6.99855597055269,9.5666727579438,-3.0676949566889));
#31459=CARTESIAN_POINT('Ctrl Pts',(-6.93930740780788,9.87310730343358,1.85842195835291));
#31460=CARTESIAN_POINT('Ctrl Pts',(-6.88005884506304,7.7966090395667,6.33599775053658));
#31461=CARTESIAN_POINT('Ctrl Pts',(-6.8208102823182,3.83835309599371,9.28434303076916));
#31462=CARTESIAN_POINT('Ctrl Pts',(-6.76156171957337,-1.04631205655837,
9.99185723914637));
#31463=CARTESIAN_POINT('Ctrl Pts',(-6.70231315682853,-5.67844360934779,
8.28777763821964));
#31464=CARTESIAN_POINT('Ctrl Pts',(-6.64306459408369,-8.94004923030717,
4.5833939134041));
#31465=CARTESIAN_POINT('Ctrl Pts',(-6.58381603133887,-10.043921122745,-0.227219026059686));
#31466=CARTESIAN_POINT('Ctrl Pts',(-6.52456746859402,-8.7236332801272,-4.98299131039099));
#31467=CARTESIAN_POINT('Ctrl Pts',(-6.46531890584919,-5.29784497783292,
-8.53608918630591));
#31468=CARTESIAN_POINT('Ctrl Pts',(-6.40607034310436,-0.593390473281026,
-10.0289514781879));
#31469=CARTESIAN_POINT('Ctrl Pts',(-6.34682178035952,4.25428232967126,-9.1012670472368));
#31470=CARTESIAN_POINT('Ctrl Pts',(-6.28757321761468,8.07515894425764,-5.9769380146219));
#31471=CARTESIAN_POINT('Ctrl Pts',(-6.22832465486986,9.94704821341236,-1.41003966104096));
#31472=CARTESIAN_POINT('Ctrl Pts',(-6.16907609212501,9.4181585968316,3.49718009982154));
#31473=CARTESIAN_POINT('Ctrl Pts',(-6.10982752938019,6.61614072987225,7.56033477090688));
#31474=CARTESIAN_POINT('Ctrl Pts',(-6.05057896663535,2.21727818813639,9.79875795405083));
#31475=CARTESIAN_POINT('Ctrl Pts',(-5.99133040389051,-2.71673755117854,
9.67219298213572));
#31476=CARTESIAN_POINT('Ctrl Pts',(-5.93208184114568,-6.99505262321808,
7.21118705928984));
#31477=CARTESIAN_POINT('Ctrl Pts',(-5.87283327840084,-9.58507039518135,
3.00971851259834));
#31478=CARTESIAN_POINT('Ctrl Pts',(-5.81358471565601,-9.8616747675781,-1.9181633882891));
#31479=CARTESIAN_POINT('Ctrl Pts',(-5.75433615291117,-7.75810564005444,
-6.38308521668124));
#31480=CARTESIAN_POINT('Ctrl Pts',(-5.69508759016634,-3.78207185624856,
-9.30741169605342));
#31481=CARTESIAN_POINT('Ctrl Pts',(-5.6358390274215,1.10678732681236,-9.98533934420192));
#31482=CARTESIAN_POINT('Ctrl Pts',(-5.57659046467667,5.7285168460572,-8.25324631585039));
#31483=CARTESIAN_POINT('Ctrl Pts',(-5.51734190193183,8.96763496184554,-4.52918350221593));
#31484=CARTESIAN_POINT('Ctrl Pts',(-5.458093339187,10.0423613697144,0.288024522786977));
#31485=CARTESIAN_POINT('Ctrl Pts',(-5.39884477644216,8.69330449815474,5.03571612663202));
#31486=CARTESIAN_POINT('Ctrl Pts',(-5.33959621369733,5.24606719772168,8.56800787596791));
#31487=CARTESIAN_POINT('Ctrl Pts',(-5.2803476509525,0.532660568335423,10.0323602768541));
#31488=CARTESIAN_POINT('Ctrl Pts',(-5.22109908820766,-4.30930683790513,
9.07534322119243));
#31489=CARTESIAN_POINT('Ctrl Pts',(-5.16185052546282,-8.11119756545325,
5.92793843252815));
#31490=CARTESIAN_POINT('Ctrl Pts',(-5.102601962718,-9.95540281331162,1.34979066168298));
#31491=CARTESIAN_POINT('Ctrl Pts',(-5.04335339997315,-9.39681274336244,
-3.55413706430132));
#31492=CARTESIAN_POINT('Ctrl Pts',(-4.98410483722832,-6.57024637095018,
-7.60025280044521));
#31493=CARTESIAN_POINT('Ctrl Pts',(-4.92485627448348,-2.1579121985799,-9.8120025962532));
#31494=CARTESIAN_POINT('Ctrl Pts',(-4.86560771173865,2.77524683886309,-9.65556756431436));
#31495=CARTESIAN_POINT('Ctrl Pts',(-4.80635914899381,7.03858364658536,-7.16870422431282));
#31496=CARTESIAN_POINT('Ctrl Pts',(-4.74711058624898,9.60311668441919,-2.95163174381379));
#31497=CARTESIAN_POINT('Ctrl Pts',(-4.68786202350415,9.8498807441029,1.97783450587003));
#31498=CARTESIAN_POINT('Ctrl Pts',(-4.62861346075931,7.71931786114931,6.42993870609979));
#31499=CARTESIAN_POINT('Ctrl Pts',(-4.56936489801447,3.72565198163625,9.33013919067606));
#31500=CARTESIAN_POINT('Ctrl Pts',(-4.51011633526964,-1.1672220268825,9.97845542885368));
#31501=CARTESIAN_POINT('Ctrl Pts',(-4.45086777252481,-5.77838009947901,
8.21841246419309));
#31502=CARTESIAN_POINT('Ctrl Pts',(-4.39161920977997,-8.99489197765177,
4.47480707025844));
#31503=CARTESIAN_POINT('Ctrl Pts',(-4.33237064703514,-10.0404335060174,
-0.348819461759353));
#31504=CARTESIAN_POINT('Ctrl Pts',(-4.2731220842903,-8.66265705625382,-5.08825635472459));
#31505=CARTESIAN_POINT('Ctrl Pts',(-4.21387352154547,-5.19409711888415,
-8.5996124985524));
#31506=CARTESIAN_POINT('Ctrl Pts',(-4.15462495880063,-0.471911138296548,
-10.0354013314471));
#31507=CARTESIAN_POINT('Ctrl Pts',(-4.0953763960558,4.3641733851008,-9.04908673129157));
#31508=CARTESIAN_POINT('Ctrl Pts',(-4.03612783331096,8.14693886431048,-5.87872155717949));
#31509=CARTESIAN_POINT('Ctrl Pts',(-3.97687927056613,9.96339249007565,-1.28949218468484));
#31510=CARTESIAN_POINT('Ctrl Pts',(-3.91763070782129,9.37512244231739,3.61096374908634));
#31511=CARTESIAN_POINT('Ctrl Pts',(-3.85838214507646,6.52411117446994,7.63989223672795));
#31512=CARTESIAN_POINT('Ctrl Pts',(-3.79913358233162,2.09846710905133,9.82488757176839));
#31513=CARTESIAN_POINT('Ctrl Pts',(-3.73988501958679,-2.83365439768783,
9.6385882140552));
#31514=CARTESIAN_POINT('Ctrl Pts',(-3.68063645684195,-7.08185666512257,
7.12595861483339));
#31515=CARTESIAN_POINT('Ctrl Pts',(-3.62138789409712,-9.62081096384753,
2.89343678064173));
#31516=CARTESIAN_POINT('Ctrl Pts',(-3.56213933135228,-9.83772566548719,
-2.03743312436855));
#31517=CARTESIAN_POINT('Ctrl Pts',(-3.50289076860745,-7.68024712456503,
-6.4765565010482));
#31518=CARTESIAN_POINT('Ctrl Pts',(-3.44364220586261,-3.6690955403147,-9.35252468169435));
#31519=CARTESIAN_POINT('Ctrl Pts',(-3.38439364311778,1.22761394150943,-9.97120574535853));
#31520=CARTESIAN_POINT('Ctrl Pts',(-3.32514508037294,5.82803154182476,-8.18327736015069));
#31521=CARTESIAN_POINT('Ctrl Pts',(-3.26589651762811,9.02181927860445,-4.42026661072162));
#31522=CARTESIAN_POINT('Ctrl Pts',(-3.20664795488328,10.0381376023182,0.409601614479463));
#31523=CARTESIAN_POINT('Ctrl Pts',(-3.14739939213844,8.6316920778322,5.14061006877085));
#31524=CARTESIAN_POINT('Ctrl Pts',(-3.08815082939361,5.14193664632369,8.63090189556414));
#31525=CARTESIAN_POINT('Ctrl Pts',(-3.02890226664877,0.411144409983018,
10.0380745304963));
#31526=CARTESIAN_POINT('Ctrl Pts',(-2.96965370390394,-4.41887996008199,
9.02249853998576));
#31527=CARTESIAN_POINT('Ctrl Pts',(-2.9104051411591,-8.18238153070373,5.82928919265959));
#31528=CARTESIAN_POINT('Ctrl Pts',(-2.85115657841427,-9.97101695083666,
1.22914644033452));
#31529=CARTESIAN_POINT('Ctrl Pts',(-2.79190801566943,-9.35308848877147,
-3.66765807114975));
#31530=CARTESIAN_POINT('Ctrl Pts',(-2.7326594529246,-6.47773683155344,-7.6792516267404));
#31531=CARTESIAN_POINT('Ctrl Pts',(-2.67341089017976,-2.03894509855726,
-9.83741240828749));
#31532=CARTESIAN_POINT('Ctrl Pts',(-2.61416232743493,2.89195808667764,-9.62125555374968));
#31533=CARTESIAN_POINT('Ctrl Pts',(-2.55491376469009,7.12487009262311,-7.08295179772558));
#31534=CARTESIAN_POINT('Ctrl Pts',(-2.49566520194526,9.63815258486866,-2.83513575626437));
#31535=CARTESIAN_POINT('Ctrl Pts',(-2.43641663920042,9.8252099772849,2.09695705915036));
#31536=CARTESIAN_POINT('Ctrl Pts',(-2.37716807645559,7.64089486247027,6.52293689271442));
#31537=CARTESIAN_POINT('Ctrl Pts',(-2.31791951371075,3.61240460540479,9.37456734855053));
#31538=CARTESIAN_POINT('Ctrl Pts',(-2.25867095096591,-1.28796085698004,
9.9635905594593));
#31539=CARTESIAN_POINT('Ctrl Pts',(-2.19942238822108,-5.87746935308181,
8.14784229162806));
#31540=CARTESIAN_POINT('Ctrl Pts',(-2.14017382547625,-9.04841587766215,
4.36556412282892));
#31541=CARTESIAN_POINT('Ctrl Pts',(-2.08092526273141,-10.035473742775,-0.470368752929598));
#31542=CARTESIAN_POINT('Ctrl Pts',(-2.02167669998658,-8.60041069793557,
-5.19277534970414));
#31543=CARTESIAN_POINT('Ctrl Pts',(-1.96242813724174,-5.08958769202351,
-8.66187492006564));
#31544=CARTESIAN_POINT('Ctrl Pts',(-1.90317957449691,-0.350362610847111,
-10.0403797760134));
#31545=CARTESIAN_POINT('Ctrl Pts',(-1.84393101175207,4.47342455753611,-8.99557962188608));
#31546=CARTESIAN_POINT('Ctrl Pts',(-1.78468244900724,8.21752426545409,-5.7796431509508));
#31547=CARTESIAN_POINT('Ctrl Pts',(-1.7254338862624,9.97827591611403,-1.16875564065287));
#31548=CARTESIAN_POINT('Ctrl Pts',(-1.66618532351757,9.3307116903966,3.72421795231635));
#31549=CARTESIAN_POINT('Ctrl Pts',(-1.60693676077273,6.43112504208883,7.71832952773314));
#31550=CARTESIAN_POINT('Ctrl Pts',(-1.5476881980279,1.97934834892384,9.84957664670273));
#31551=CARTESIAN_POINT('Ctrl Pts',(-1.48843963528306,-2.9501557686649,9.60357021874013));
#31552=CARTESIAN_POINT('Ctrl Pts',(-1.42919107253823,-7.16762235239588,
7.03968534943816));
#31553=CARTESIAN_POINT('Ctrl Pts',(-1.36994250979339,-9.65514091181178,
2.77673080775176));
#31554=CARTESIAN_POINT('Ctrl Pts',(-1.31069394704856,-9.81233413826848,
-2.15640412831874));
#31555=CARTESIAN_POINT('Ctrl Pts',(-1.25144538430372,-7.60126251735319,
-6.56907818098861));
#31556=CARTESIAN_POINT('Ctrl Pts',(-1.19219682155889,-3.5555812549575,-9.39626638325325));
#31557=CARTESIAN_POINT('Ctrl Pts',(-1.13294825881405,1.34826056123045,-9.95561015029659));
#31558=CARTESIAN_POINT('Ctrl Pts',(-1.07369969606922,5.9266917210682,-8.11210855752574));
#31559=CARTESIAN_POINT('Ctrl Pts',(-1.01445113332438,9.07468079990562,-4.31070161174287));
#31560=CARTESIAN_POINT('Ctrl Pts',(-0.955202570579551,10.0324420250335,
0.531118649642064));
#31561=CARTESIAN_POINT('Ctrl Pts',(-0.895954007834716,8.5688140632078,5.24475028536576));
#31562=CARTESIAN_POINT('Ctrl Pts',(-0.836705445089879,5.03705217487539,
8.6925304367147));
#31563=CARTESIAN_POINT('Ctrl Pts',(-0.777456882345046,0.289567968894557,
10.0423169835008));
#31564=CARTESIAN_POINT('Ctrl Pts',(-0.71820831960021,-4.52780517808973,
8.96833096372111));
#31565=CARTESIAN_POINT('Ctrl Pts',(-0.658959756855376,-8.25236578037355,
5.72978525187863));
#31566=CARTESIAN_POINT('Ctrl Pts',(-0.59971119411054,-9.9851691198313,1.10832199929135));
#31567=CARTESIAN_POINT('Ctrl Pts',(-0.540462631365706,-9.30799286741916,
-3.78064131929891));
#31568=CARTESIAN_POINT('Ctrl Pts',(-0.481214068620872,-6.38427751469271,
-7.75712450735258));
#31569=CARTESIAN_POINT('Ctrl Pts',(-0.421965505876037,-1.91967904466917,
-9.86137984097431));
#31570=CARTESIAN_POINT('Ctrl Pts',(-0.3627169431312,3.00824531027549,-9.58553285758615));
#31571=CARTESIAN_POINT('Ctrl Pts',(-0.303468380386366,7.21011187750129,
-6.99616085537751));
#31572=CARTESIAN_POINT('Ctrl Pts',(-0.24421981764153,9.67177532161258,-2.71822407706291));
#31573=CARTESIAN_POINT('Ctrl Pts',(-0.184971254896697,9.7990986210757,2.21577215487913));
#31574=CARTESIAN_POINT('Ctrl Pts',(-0.125722692151862,7.56135154068707,
6.61497867050113));
#31575=CARTESIAN_POINT('Ctrl Pts',(-0.0664741294070281,3.49862757435156,
9.41762099817694));
#31576=CARTESIAN_POINT('Ctrl Pts',(-0.00722556666219214,-1.40851084870404,
9.94726479539839));
#31577=CARTESIAN_POINT('Ctrl Pts',(0.0520229960826427,-5.97569683227752,
8.07607749665164));
#31578=CARTESIAN_POINT('Ctrl Pts',(0.111271558827478,-9.10061310037694,
4.25568103258189));
#31579=CARTESIAN_POINT('Ctrl Pts',(0.170520121572313,-10.029042525852,-0.591848969840164));
#31580=CARTESIAN_POINT('Ctrl Pts',(0.229768684317147,-8.53690339820701,
-5.29653317896745));
#31581=CARTESIAN_POINT('Ctrl Pts',(0.289017247061983,-4.98433189249667,
-8.72286691948016));
#31582=CARTESIAN_POINT('Ctrl Pts',(0.348265809806816,-0.228762959938813,
-10.0438868586929));
#31583=CARTESIAN_POINT('Ctrl Pts',(0.407514372551653,4.58202030589382,-8.94075206471425));
#31584=CARTESIAN_POINT('Ctrl Pts',(0.466762935296486,8.28690387641807,-5.67972021817628));
#31585=CARTESIAN_POINT('Ctrl Pts',(0.526011498041321,9.991698089155,-1.0478421420499));
#31586=CARTESIAN_POINT('Ctrl Pts',(0.585260060786157,9.28492941638948,3.83691531271406));
#31587=CARTESIAN_POINT('Ctrl Pts',(0.644508623530991,6.3372026009131,7.79565597764807));
#31588=CARTESIAN_POINT('Ctrl Pts',(0.703757186275827,1.85992656207777,9.87278133064767));
#31589=CARTESIAN_POINT('Ctrl Pts',(0.76300574902066,-3.06619982410485,9.56722184472157));
#31590=CARTESIAN_POINT('Ctrl Pts',(0.822254311765497,-7.25238514954131,
6.95222940819188));
#31591=CARTESIAN_POINT('Ctrl Pts',(0.881502874510329,-9.6879601464798,2.65991277096996));
#31592=CARTESIAN_POINT('Ctrl Pts',(0.940751437255167,-9.7857096158956,-2.27567180872784));
#31593=CARTESIAN_POINT('Ctrl Pts',(0.980250479085055,-8.27561480792394,
-5.19792551867508));
#31594=CARTESIAN_POINT('Ctrl Pts',(1.,-7.218010097054,-6.39216838336776));
#31595=CARTESIAN_POINT('Ctrl Pts',(1.,-7.218010097054,-6.39216838336776));
#31596=CARTESIAN_POINT('Ctrl Pts',(1.,-7.38033772502723,-6.21660074016268));
#31597=CARTESIAN_POINT('Ctrl Pts',(0.999999999999999,-7.53570865858123,
-6.03520929800804));
#31598=CARTESIAN_POINT('Ctrl Pts',(0.999999999999999,-7.68398068614723,
-5.84850759966542));
#31599=CARTESIAN_POINT('Ctrl Pts',(1.,-7.83425301467726,-5.65928715524971));
#31600=CARTESIAN_POINT('Ctrl Pts',(1.,-7.97723397958538,-5.46461174998116));
#31601=CARTESIAN_POINT('Ctrl Pts',(1.,-8.11274192803781,-5.26497371679585));
#31602=CARTESIAN_POINT('Ctrl Pts',(1.,-8.24926802235148,-5.06383569309665));
#31603=CARTESIAN_POINT('Ctrl Pts',(0.999999999999998,-8.37820875008256,
-4.85765966198851));
#31604=CARTESIAN_POINT('Ctrl Pts',(0.999999999999998,-8.49933886135329,
-4.64691404211075));
#31605=CARTESIAN_POINT('Ctrl Pts',(0.999999999999997,-8.62014279896438,
-4.43673590846219));
#31606=CARTESIAN_POINT('Ctrl Pts',(1.,-8.73317843953205,-4.22201218564418));
#31607=CARTESIAN_POINT('Ctrl Pts',(1.,-8.83817822275541,-4.00318110377646));
#31608=CARTESIAN_POINT('Ctrl Pts',(1.,-8.90711959723496,-3.85949970654237));
#31609=CARTESIAN_POINT('Ctrl Pts',(1.,-8.97259576417475,-3.71404708405175));
#31610=CARTESIAN_POINT('Ctrl Pts',(1.,-9.03451959595587,-3.56694287159514));
#31611=CARTESIAN_POINT('Ctrl Pts',(1.,-9.06021095437682,-3.50591132786227));
#31612=CARTESIAN_POINT('Ctrl Pts',(1.,-9.08529073461529,-3.44459546100671));
#31613=CARTESIAN_POINT('Ctrl Pts',(1.,-9.10975222670468,-3.38300368933708));
#31614=CARTESIAN_POINT('Ctrl Pts',(1.,-9.12543439611011,-3.34351743912086));
#31615=CARTESIAN_POINT('Ctrl Pts',(0.999999999999998,-9.1408624405508,-3.30391778949324));
#31616=CARTESIAN_POINT('Ctrl Pts',(0.999999999999998,-9.15603452786866,
-3.26420694634604));
#31617=CARTESIAN_POINT('Ctrl Pts',(0.999999999999998,-9.16539765652395,
-3.23970025022654));
#31618=CARTESIAN_POINT('Ctrl Pts',(1.,-9.17466411167333,-3.21514903349331));
#31619=CARTESIAN_POINT('Ctrl Pts',(1.,-9.18383080790029,-3.19056092275229));
#31620=CARTESIAN_POINT('Ctrl Pts',(1.,-9.26956815148778,-2.96058501359442));
#31621=CARTESIAN_POINT('Ctrl Pts',(1.,-9.34642884496221,-2.72779994416276));
#31622=CARTESIAN_POINT('Ctrl Pts',(1.,-9.41421857063004,-2.492691400286));
#31623=CARTESIAN_POINT('Ctrl Pts',(1.,-9.4415819795859,-2.39778953762557));
#31624=CARTESIAN_POINT('Ctrl Pts',(1.,-9.46746693113579,-2.30250875679181));
#31625=CARTESIAN_POINT('Ctrl Pts',(1.,-9.49185860296011,-2.20687973654423));
#31626=CARTESIAN_POINT('Ctrl Pts',(1.,-9.55185343242315,-1.97166638984157));
#31627=CARTESIAN_POINT('Ctrl Pts',(1.,-9.60281768869445,-1.7343475047727));
#31628=CARTESIAN_POINT('Ctrl Pts',(1.,-9.64482604864012,-1.49544925869656));
#31629=CARTESIAN_POINT('Ctrl Pts',(1.,-9.6871492900488,-1.25476030645304));
#31630=CARTESIAN_POINT('Ctrl Pts',(1.,-9.72038194639541,-1.01246759088605));
#31631=CARTESIAN_POINT('Ctrl Pts',(1.,-9.74454903488948,-0.769095725160656));
#31632=CARTESIAN_POINT('Ctrl Pts',(1.,-9.76872045220789,-0.525680266511232));
#31633=CARTESIAN_POINT('Ctrl Pts',(1.,-9.78382307936487,-0.28118460779274));
#31634=CARTESIAN_POINT('Ctrl Pts',(1.,-9.78983010083248,-0.0361300070823768));
#31635=CARTESIAN_POINT('Ctrl Pts',(1.,-9.79255545728033,0.0750500743810585));
#31636=CARTESIAN_POINT('Ctrl Pts',(1.,-9.79340787224445,0.186345196742594));
#31637=CARTESIAN_POINT('Ctrl Pts',(1.,-9.79238129738034,0.29770636029337));
#31638=CARTESIAN_POINT('Ctrl Pts',(1.,-9.7918485179152,0.355501405961876));
#31639=CARTESIAN_POINT('Ctrl Pts',(1.,-9.79080959995854,0.413314234074637));
#31640=CARTESIAN_POINT('Ctrl Pts',(1.,-9.78926346177246,0.471137948752055));
#31641=CARTESIAN_POINT('Ctrl Pts',(1.,-9.78827695465579,0.508032132308922));
#31642=CARTESIAN_POINT('Ctrl Pts',(1.,-9.78708370731581,0.544935718081712));
#31643=CARTESIAN_POINT('Ctrl Pts',(1.,-9.78568473007052,0.581816524025753));
#31644=CARTESIAN_POINT('Ctrl Pts',(1.,-9.7763473698279,0.827974474268892));
#31645=CARTESIAN_POINT('Ctrl Pts',(0.999999999999998,-9.75784570194124,
1.07334621400395));
#31646=CARTESIAN_POINT('Ctrl Pts',(0.999999999999998,-9.730258741531,1.3174026125394));
#31647=CARTESIAN_POINT('Ctrl Pts',(0.999999999999998,-9.70256575117013,
1.56239703713871));
#31648=CARTESIAN_POINT('Ctrl Pts',(0.999999999999996,-9.66571752447539,
1.80606665550865));
#31649=CARTESIAN_POINT('Ctrl Pts',(0.999999999999996,-9.61974203609876,
2.04788259603852));
#31650=CARTESIAN_POINT('Ctrl Pts',(0.999999999999996,-9.58407738698297,
2.23546691485976));
#31651=CARTESIAN_POINT('Ctrl Pts',(0.999999999999998,-9.54291928114351,
2.42193598770508));
#31652=CARTESIAN_POINT('Ctrl Pts',(0.999999999999999,-9.4962591980495,2.60704169439268));
#31653=CARTESIAN_POINT('Ctrl Pts',(0.999999999999999,-9.4361780998623,2.84539005129771));
#31654=CARTESIAN_POINT('Ctrl Pts',(1.,-9.36697631765938,3.08147877897739));
#31655=CARTESIAN_POINT('Ctrl Pts',(1.,-9.28891866527466,3.31486192371426));
#31656=CARTESIAN_POINT('Ctrl Pts',(1.,-9.2337641129153,3.47976750930297));
#31657=CARTESIAN_POINT('Ctrl Pts',(0.999999999999998,-9.17418703363605,
3.64332206604504));
#31658=CARTESIAN_POINT('Ctrl Pts',(0.999999999999998,-9.1102663177799,3.8053623967777));
#31659=CARTESIAN_POINT('Ctrl Pts',(0.999999999999998,-9.07823122598397,
3.88657201403772));
#31660=CARTESIAN_POINT('Ctrl Pts',(1.,-9.04510495830855,3.96740121333635));
#31661=CARTESIAN_POINT('Ctrl Pts',(1.,-9.01089637781328,4.04782884761811));
#31662=CARTESIAN_POINT('Ctrl Pts',(1.,-8.98491018784549,4.1089248578251));
#31663=CARTESIAN_POINT('Ctrl Pts',(0.999999999999997,-8.95829943234446,
4.16978913592025));
#31664=CARTESIAN_POINT('Ctrl Pts',(0.999999999999996,-8.93106773262397,
4.23041223277627));
#31665=CARTESIAN_POINT('Ctrl Pts',(0.999999999999996,-8.91985573978134,
4.2553723246921));
#31666=CARTESIAN_POINT('Ctrl Pts',(1.,-8.90854184623664,4.28028401514663));
#31667=CARTESIAN_POINT('Ctrl Pts',(1.,-8.89712824313656,4.30514296030326));
#31668=CARTESIAN_POINT('Ctrl Pts',(1.,-8.79449431220153,4.52868071940972));
#31669=CARTESIAN_POINT('Ctrl Pts',(0.999999999999998,-8.68375800201423,
4.74805239366863));
#31670=CARTESIAN_POINT('Ctrl Pts',(0.999999999999999,-8.56525007473062,
4.96284307910226));
#31671=CARTESIAN_POINT('Ctrl Pts',(0.999999999999999,-8.44538160194408,
5.18009969662868));
#31672=CARTESIAN_POINT('Ctrl Pts',(0.999999999999999,-8.31756182226729,
5.39267013902898));
#31673=CARTESIAN_POINT('Ctrl Pts',(0.999999999999999,-8.18208200192093,
5.60011072880211));
#31674=CARTESIAN_POINT('Ctrl Pts',(0.999999999999999,-8.04666336029153,
5.80745764448343));
#31675=CARTESIAN_POINT('Ctrl Pts',(1.,-7.90359128193536,6.00967992523946));
#31676=CARTESIAN_POINT('Ctrl Pts',(1.,-7.75311011393737,6.20631136198203));
#31677=CARTESIAN_POINT('Ctrl Pts',(1.,-7.60409271693618,6.40103011158911));
#31678=CARTESIAN_POINT('Ctrl Pts',(1.,-7.44780931337785,6.59026678062805));
#31679=CARTESIAN_POINT('Ctrl Pts',(1.,-7.28445663684239,6.77353773959716));
#31680=CARTESIAN_POINT('Ctrl Pts',(1.,-7.25089458908372,6.81119214972472));
#31681=CARTESIAN_POINT('Ctrl Pts',(1.,-7.2170339997554,6.84859461006606));
#31682=CARTESIAN_POINT('Ctrl Pts',(1.,-7.18287638116905,6.88574073117186));
#31683=CARTESIAN_POINT('Ctrl Pts',(1.,-7.04310063062746,7.03774567683707));
#31684=CARTESIAN_POINT('Ctrl Pts',(1.,-6.89835224551882,7.18545977217479));
#31685=CARTESIAN_POINT('Ctrl Pts',(1.,-6.74886883975424,7.32870626947399));
#31686=CARTESIAN_POINT('Ctrl Pts',(1.,-6.72044540624219,7.35594378972577));
#31687=CARTESIAN_POINT('Ctrl Pts',(1.,-6.69184773627237,7.3830224478866));
#31688=CARTESIAN_POINT('Ctrl Pts',(1.,-6.66309768238747,7.4099222241242));
#31689=CARTESIAN_POINT('Ctrl Pts',(1.,-6.48228040589527,7.57910257755957));
#31690=CARTESIAN_POINT('Ctrl Pts',(1.,-6.29529510224086,7.74135043073779));
#31691=CARTESIAN_POINT('Ctrl Pts',(1.,-6.10262676105486,7.89643853847066));
#31692=CARTESIAN_POINT('Ctrl Pts',(1.,-5.90856004843239,8.05265226330623));
#31693=CARTESIAN_POINT('Ctrl Pts',(1.,-5.70872700746814,8.20160234411627));
#31694=CARTESIAN_POINT('Ctrl Pts',(1.,-5.50358541811632,8.34301973665858));
#31695=CARTESIAN_POINT('Ctrl Pts',(1.,-5.3158480140083,8.47243929636612));
#31696=CARTESIAN_POINT('Ctrl Pts',(0.999999999999999,-5.12366386476961,
8.59554989096275));
#31697=CARTESIAN_POINT('Ctrl Pts',(0.999999999999999,-4.92736180550962,
8.71211419861635));
#31698=CARTESIAN_POINT('Ctrl Pts',(0.999999999999999,-4.89295954817348,
8.73254228441038));
#31699=CARTESIAN_POINT('Ctrl Pts',(1.,-4.85843077260399,8.75276923386899));
#31700=CARTESIAN_POINT('Ctrl Pts',(1.,-4.82377719504876,8.77279366648196));
#31701=CARTESIAN_POINT('Ctrl Pts',(1.,-4.79450813505122,8.78970667693901));
#31702=CARTESIAN_POINT('Ctrl Pts',(0.999999999999996,-4.76515157312949,
8.80647428626319));
#31703=CARTESIAN_POINT('Ctrl Pts',(0.999999999999996,-4.73571877009977,
8.82309006334544));
#31704=CARTESIAN_POINT('Ctrl Pts',(0.999999999999997,-4.51751740444002,
8.94627184957165));
#31705=CARTESIAN_POINT('Ctrl Pts',(1.,-4.29497551340846,9.06120098158676));
#31706=CARTESIAN_POINT('Ctrl Pts',(0.999999999999999,-4.06855850342775,
9.16761502395632));
#31707=CARTESIAN_POINT('Ctrl Pts',(0.999999999999999,-3.84298106373966,
9.27363447552769));
#31708=CARTESIAN_POINT('Ctrl Pts',(1.,-3.61355662653113,9.37120220887847));
#31709=CARTESIAN_POINT('Ctrl Pts',(1.,-3.38071834466137,9.46001497115018));
#31710=CARTESIAN_POINT('Ctrl Pts',(1.,-3.27719789143318,9.4995013362315));
#31711=CARTESIAN_POINT('Ctrl Pts',(0.999999999999997,-3.17300231116554,
9.53725648506412));
#31712=CARTESIAN_POINT('Ctrl Pts',(0.999999999999997,-3.06816838561069,
9.57325070271326));
#31713=CARTESIAN_POINT('Ctrl Pts',(0.999999999999997,-2.91468505697523,
9.62594845591844));
#31714=CARTESIAN_POINT('Ctrl Pts',(0.999999999999999,-2.75983351721763,
9.67487209480759));
#31715=CARTESIAN_POINT('Ctrl Pts',(0.999999999999999,-2.60375578640692,
9.7200109471421));
#31716=CARTESIAN_POINT('Ctrl Pts',(0.16348406216194,-9.64208031777467,-0.000174349252608778));
#31717=CARTESIAN_POINT('Ctrl Pts',(0.165829415298731,-9.64223943100266,
-0.189581381928583));
#31718=CARTESIAN_POINT('Ctrl Pts',(0.168174768435523,-9.63677165214438,
-0.378979236144793));
#31719=CARTESIAN_POINT('Ctrl Pts',(0.170520121572314,-9.62561443366536,
-0.568041337624323));
#31720=CARTESIAN_POINT('Ctrl Pts',(0.19026964248726,-9.53166281663704,-2.16007703954927));
#31721=CARTESIAN_POINT('Ctrl Pts',(0.210019163402205,-9.034283107422,-3.72830510925844));
#31722=CARTESIAN_POINT('Ctrl Pts',(0.229768684317151,-8.19349800186272,
-5.0834747675318));
#31723=CARTESIAN_POINT('Ctrl Pts',(0.249518205232095,-7.35271289630349,
-6.43864442580509));
#31724=CARTESIAN_POINT('Ctrl Pts',(0.26926772614704,-6.16852239440005,-7.58075567264264));
#31725=CARTESIAN_POINT('Ctrl Pts',(0.289017247061984,-4.78383232135538,
-8.37198128593018));
#31726=CARTESIAN_POINT('Ctrl Pts',(0.308766767976929,-3.39914224831071,
-9.16320689921773));
#31727=CARTESIAN_POINT('Ctrl Pts',(0.328516288891873,-1.81395260412477,
-9.60354687895529));
#31728=CARTESIAN_POINT('Ctrl Pts',(0.348265809806818,-0.219560571059729,
-9.63986106982765));
#31729=CARTESIAN_POINT('Ctrl Pts',(0.368015330721763,1.37483146200536,-9.6761752607));
#31730=CARTESIAN_POINT('Ctrl Pts',(0.387764851636707,2.97842588394947,-9.30846366270717));
#31731=CARTESIAN_POINT('Ctrl Pts',(0.407514372551652,4.39770369000897,-8.58110255595442));
#31732=CARTESIAN_POINT('Ctrl Pts',(0.427263893466598,5.81698149606851,-7.85374144920165));
#31733=CARTESIAN_POINT('Ctrl Pts',(0.447013414381543,7.05194268624332,-6.76673083368895));
#31734=CARTESIAN_POINT('Ctrl Pts',(0.466762935296488,7.95355565012021,-5.45124584657818));
#31735=CARTESIAN_POINT('Ctrl Pts',(0.486512456211433,8.85516861399705,-4.13576085946748));
#31736=CARTESIAN_POINT('Ctrl Pts',(0.506261977126377,9.42343335157602,-2.5918015007587));
#31737=CARTESIAN_POINT('Ctrl Pts',(0.526011498041322,9.58977094157126,-1.00569557894368));
#31738=CARTESIAN_POINT('Ctrl Pts',(0.545761018956267,9.7561085315665,0.580410342871385));
#31739=CARTESIAN_POINT('Ctrl Pts',(0.565510539871213,9.52051897397799,2.20866282779273));
#31740=CARTESIAN_POINT('Ctrl Pts',(0.585260060786158,8.91143639260434,3.68257918107574));
#31741=CARTESIAN_POINT('Ctrl Pts',(0.605009581701103,8.30235381123068,5.15649553435874));
#31742=CARTESIAN_POINT('Ctrl Pts',(0.624759102616048,7.31977820607187,6.47607575600343));
#31743=CARTESIAN_POINT('Ctrl Pts',(0.644508623530993,6.08227773035324,7.48205342565903));
#31744=CARTESIAN_POINT('Ctrl Pts',(0.664258144445937,4.84477725463465,8.48803109531461));
#31745=CARTESIAN_POINT('Ctrl Pts',(0.684007665360883,3.35235190835623,9.18040621298113));
#31746=CARTESIAN_POINT('Ctrl Pts',(0.703757186275827,1.78511817085327,9.47566719082672));
#31747=CARTESIAN_POINT('Ctrl Pts',(0.723506707190773,0.217884433350224,
9.77092816867232));
#31748=CARTESIAN_POINT('Ctrl Pts',(0.743256228105716,-1.42415769537726,
9.66907500669695));
#31749=CARTESIAN_POINT('Ctrl Pts',(0.763005749020662,-2.94287631398048,
9.18231635295431));
#31750=CARTESIAN_POINT('Ctrl Pts',(0.782755269935607,-4.46159493258366,
8.69555769921168));
#31751=CARTESIAN_POINT('Ctrl Pts',(0.802504790850553,-5.8569900410625,7.82389355370177));
#31752=CARTESIAN_POINT('Ctrl Pts',(0.822254311765498,-6.96061676145832,
6.67267537474318));
#31753=CARTESIAN_POINT('Ctrl Pts',(0.842003832680442,-8.06424348185414,
5.52145719578458));
#31754=CARTESIAN_POINT('Ctrl Pts',(0.861753353595387,-8.87610181416697,
4.09068498337726));
#31755=CARTESIAN_POINT('Ctrl Pts',(0.881502874510331,-9.29832255855935,
2.55270144722397));
#31756=CARTESIAN_POINT('Ctrl Pts',(0.892163270394199,-9.52622886094455,
1.72252873423131));
#31757=CARTESIAN_POINT('Ctrl Pts',(0.902823666278068,-9.64060941270616,
0.861118670477449));
#31758=CARTESIAN_POINT('Ctrl Pts',(0.913484062161936,-9.64080718149228,
-0.000193112876372633));
#31759=CARTESIAN_POINT('Ctrl Pts',(-8.,-2.60344811511687,9.71940883564398));
#31760=CARTESIAN_POINT('Ctrl Pts',(-8.,-2.84069175470075,9.6506071796457));
#31761=CARTESIAN_POINT('Ctrl Pts',(-8.,-3.07490729689743,9.57303453428213));
#31762=CARTESIAN_POINT('Ctrl Pts',(-8.,-3.30569495421949,9.4870393850882));
#31763=CARTESIAN_POINT('Ctrl Pts',(-8.,-3.53907133521668,9.40007963630845));
#31764=CARTESIAN_POINT('Ctrl Pts',(-8.,-3.76894306703271,9.30450711868265));
#31765=CARTESIAN_POINT('Ctrl Pts',(-8.,-3.9948840188511,9.20063005080582));
#31766=CARTESIAN_POINT('Ctrl Pts',(-8.,-4.22183166262119,9.09629015311723));
#31767=CARTESIAN_POINT('Ctrl Pts',(-8.,-4.44481399609299,8.98357122395935));
#31768=CARTESIAN_POINT('Ctrl Pts',(-8.,-4.66337776867861,8.86273771780899));
#31769=CARTESIAN_POINT('Ctrl Pts',(-8.,-4.88031678224955,8.74280246357875));
#31770=CARTESIAN_POINT('Ctrl Pts',(-8.,-5.09290319963608,8.61487244542648));
#31771=CARTESIAN_POINT('Ctrl Pts',(-8.,-5.30066469035802,8.47916451832081));
#31772=CARTESIAN_POINT('Ctrl Pts',(-8.,-5.43935748628783,8.3885716381161));
#31773=CARTESIAN_POINT('Ctrl Pts',(-8.,-5.57589952659966,8.29451181350657));
#31774=CARTESIAN_POINT('Ctrl Pts',(-8.,-5.71014126262514,8.19704032519922));
#31775=CARTESIAN_POINT('Ctrl Pts',(-8.,-5.81242682170959,8.12277187507713));
#31776=CARTESIAN_POINT('Ctrl Pts',(-8.,-5.91337675491332,8.04652256746091));
#31777=CARTESIAN_POINT('Ctrl Pts',(-8.,-6.01292162257584,7.96831424157311));
#31778=CARTESIAN_POINT('Ctrl Pts',(-8.,-6.03974603533308,7.94723939900283));
#31779=CARTESIAN_POINT('Ctrl Pts',(-8.,-6.06647083477937,7.92602027127446));
#31780=CARTESIAN_POINT('Ctrl Pts',(-8.,-6.09307507746351,7.9046731501823));
#31781=CARTESIAN_POINT('Ctrl Pts',(-8.,-6.28715186618783,7.74894683392287));
#31782=CARTESIAN_POINT('Ctrl Pts',(-8.,-6.47502703975548,7.58624877613549));
#31783=CARTESIAN_POINT('Ctrl Pts',(-8.,-6.65627736318776,7.41686224654094));
#31784=CARTESIAN_POINT('Ctrl Pts',(-8.,-6.72100538512745,7.35637101653228));
#31785=CARTESIAN_POINT('Ctrl Pts',(-8.,-6.78488825702186,7.29502636554285));
#31786=CARTESIAN_POINT('Ctrl Pts',(-8.,-6.84790578274569,7.23283987189571));
#31787=CARTESIAN_POINT('Ctrl Pts',(-8.,-7.02385876529317,7.05920723707383));
#31788=CARTESIAN_POINT('Ctrl Pts',(-8.,-7.1930682957411,6.87901432974266));
#31789=CARTESIAN_POINT('Ctrl Pts',(-8.,-7.35530118613631,6.69274140140207));
#31790=CARTESIAN_POINT('Ctrl Pts',(-8.,-7.51824283162384,6.50565469303081));
#31791=CARTESIAN_POINT('Ctrl Pts',(-8.,-7.67414710687603,6.31243416749467));
#31792=CARTESIAN_POINT('Ctrl Pts',(-8.,-7.82273680022787,6.1135333512058));
#31793=CARTESIAN_POINT('Ctrl Pts',(-8.,-7.97083957648109,5.91528431773037));
#31794=CARTESIAN_POINT('Ctrl Pts',(-8.,-8.11167594519281,5.71139157758446));
#31795=CARTESIAN_POINT('Ctrl Pts',(-8.,-8.24492583126938,5.50228004576333));
#31796=CARTESIAN_POINT('Ctrl Pts',(-8.,-8.30521404253229,5.40766863123126));
#31797=CARTESIAN_POINT('Ctrl Pts',(-8.,-8.36394860502083,5.31198862209827));
#31798=CARTESIAN_POINT('Ctrl Pts',(-8.,-8.42109652453534,5.21527822770044));
#31799=CARTESIAN_POINT('Ctrl Pts',(-8.,-8.45087437095415,5.16488571479801));
#31800=CARTESIAN_POINT('Ctrl Pts',(-8.,-8.48022139245109,5.1142134322457));
#31801=CARTESIAN_POINT('Ctrl Pts',(-8.,-8.50913268358154,5.06326672997545));
#31802=CARTESIAN_POINT('Ctrl Pts',(-8.,-8.52853358179917,5.02907898717248));
#31803=CARTESIAN_POINT('Ctrl Pts',(-8.,-8.54774116172179,4.99476229317982));
#31804=CARTESIAN_POINT('Ctrl Pts',(-8.,-8.566737596633,4.96034817438508));
#31805=CARTESIAN_POINT('Ctrl Pts',(-8.,-8.68625360214662,4.74383186325392));
#31806=CARTESIAN_POINT('Ctrl Pts',(-8.,-8.79751972018929,4.52328352045298));
#31807=CARTESIAN_POINT('Ctrl Pts',(-8.,-8.90031166290089,4.29917501917082));
#31808=CARTESIAN_POINT('Ctrl Pts',(-8.,-9.00301013530597,4.07527030322198));
#31809=CARTESIAN_POINT('Ctrl Pts',(-8.,-9.09725014289365,3.8478113152238));
#31810=CARTESIAN_POINT('Ctrl Pts',(-8.,-9.18276362084067,3.61724207015639));
#31811=CARTESIAN_POINT('Ctrl Pts',(-8.,-9.25013085907205,3.43560037303228));
#31812=CARTESIAN_POINT('Ctrl Pts',(-8.,-9.3120813902539,3.2520277614531));
#31813=CARTESIAN_POINT('Ctrl Pts',(-8.,-9.36846282230467,3.06673324765561));
#31814=CARTESIAN_POINT('Ctrl Pts',(-8.,-9.44021345233254,2.83092869956063));
#31815=CARTESIAN_POINT('Ctrl Pts',(-8.,-9.50294661414108,2.59233538545246));
#31816=CARTESIAN_POINT('Ctrl Pts',(-8.,-9.55662994873875,2.35147811162457));
#31817=CARTESIAN_POINT('Ctrl Pts',(-8.,-9.59403316915113,2.18366369084712));
#31818=CARTESIAN_POINT('Ctrl Pts',(-8.,-9.62704213125647,2.01475001121834));
#31819=CARTESIAN_POINT('Ctrl Pts',(-8.,-9.65563094000264,1.84491408895825));
#31820=CARTESIAN_POINT('Ctrl Pts',(-8.,-9.66985498260186,1.76041412204629));
#31821=CARTESIAN_POINT('Ctrl Pts',(-8.,-9.68298464758163,1.67568586609032));
#31822=CARTESIAN_POINT('Ctrl Pts',(-8.,-9.6950156054378,1.59075123501256));
#31823=CARTESIAN_POINT('Ctrl Pts',(-8.,-9.70329987511925,1.53226699813347));
#31824=CARTESIAN_POINT('Ctrl Pts',(-8.,-9.71106318630873,1.47368491207996));
#31825=CARTESIAN_POINT('Ctrl Pts',(-8.,-9.71830391560107,1.41501216875315));
#31826=CARTESIAN_POINT('Ctrl Pts',(-8.,-9.72177711672372,1.38686828575954));
#31827=CARTESIAN_POINT('Ctrl Pts',(-8.,-9.7251301421797,1.35870260813857));
#31828=CARTESIAN_POINT('Ctrl Pts',(-8.,-9.72836100509793,1.33053262617027));
#31829=CARTESIAN_POINT('Ctrl Pts',(-8.,-9.75621794121566,1.08764723982277));
#31830=CARTESIAN_POINT('Ctrl Pts',(-8.,-9.77503407585364,0.844154007688625));
#31831=CARTESIAN_POINT('Ctrl Pts',(-8.,-9.78485423076769,0.600570555568447));
#31832=CARTESIAN_POINT('Ctrl Pts',(-8.,-9.7947445628712,0.35524639750051));
#31833=CARTESIAN_POINT('Ctrl Pts',(-8.,-9.79550994101194,0.109830070692749));
#31834=CARTESIAN_POINT('Ctrl Pts',(-8.,-9.78714425198491,-0.135157548107968));
#31835=CARTESIAN_POINT('Ctrl Pts',(-8.,-9.77880540331052,-0.379359152264971));
#31836=CARTESIAN_POINT('Ctrl Pts',(-8.,-9.76139396821941,-0.623135449836081));
#31837=CARTESIAN_POINT('Ctrl Pts',(-8.,-9.73485231894389,-0.865968566157455));
#31838=CARTESIAN_POINT('Ctrl Pts',(-8.,-9.70865278207418,-1.10567165009949));
#31839=CARTESIAN_POINT('Ctrl Pts',(-8.,-9.67355679806456,-1.34445630895454));
#31840=CARTESIAN_POINT('Ctrl Pts',(-8.,-9.62945950106302,-1.58181321655475));
#31841=CARTESIAN_POINT('Ctrl Pts',(-8.,-9.61925297631356,-1.63675057817564));
#31842=CARTESIAN_POINT('Ctrl Pts',(-8.,-9.60856403154122,-1.69161138395428));
#31843=CARTESIAN_POINT('Ctrl Pts',(-8.,-9.59739098933044,-1.74638917930737));
#31844=CARTESIAN_POINT('Ctrl Pts',(-8.,-9.55734323407315,-1.94273031008005));
#31845=CARTESIAN_POINT('Ctrl Pts',(-8.,-9.51107764561208,-2.13800587130263));
#31846=CARTESIAN_POINT('Ctrl Pts',(-8.,-9.45868909970552,-2.33194442065493));
#31847=CARTESIAN_POINT('Ctrl Pts',(-8.,-9.44806059824241,-2.37129035247791));
#31848=CARTESIAN_POINT('Ctrl Pts',(-8.,-9.43717863430331,-2.41058583297454));
#31849=CARTESIAN_POINT('Ctrl Pts',(-8.,-9.42605224583319,-2.44979983523773));
#31850=CARTESIAN_POINT('Ctrl Pts',(-8.,-9.35956117403027,-2.68414191732166));
#31851=CARTESIAN_POINT('Ctrl Pts',(-8.,-9.28429949582149,-2.91575310001084));
#31852=CARTESIAN_POINT('Ctrl Pts',(-8.,-9.20053845138115,-3.14417928716639));
#31853=CARTESIAN_POINT('Ctrl Pts',(-8.,-9.11644481764174,-3.37351248432862));
#31854=CARTESIAN_POINT('Ctrl Pts',(-8.,-9.02378391065593,-3.59963594961518));
#31855=CARTESIAN_POINT('Ctrl Pts',(-8.,-8.92278109081723,-3.82207193311861));
#31856=CARTESIAN_POINT('Ctrl Pts',(-8.,-8.83217822033651,-4.02160436831));
#31857=CARTESIAN_POINT('Ctrl Pts',(-8.,-8.73486208468608,-4.21816966332805));
#31858=CARTESIAN_POINT('Ctrl Pts',(-8.,-8.63096467988468,-4.41140451002018));
#31859=CARTESIAN_POINT('Ctrl Pts',(-8.,-8.6132277370607,-4.44439277795555));
#31860=CARTESIAN_POINT('Ctrl Pts',(-8.,-8.59529892556715,-4.47728393468828));
#31861=CARTESIAN_POINT('Ctrl Pts',(-8.,-8.57717882354457,-4.51007610976465));
#31862=CARTESIAN_POINT('Ctrl Pts',(-8.,-8.56101088203111,-4.5393354355716));
#31863=CARTESIAN_POINT('Ctrl Pts',(-8.,-8.54469193487426,-4.56851355146286));
#31864=CARTESIAN_POINT('Ctrl Pts',(-8.,-8.52822778415311,-4.59759995652038));
#31865=CARTESIAN_POINT('Ctrl Pts',(-8.,-8.40828066692113,-4.80950462724276));
#31866=CARTESIAN_POINT('Ctrl Pts',(-8.,-8.28055244077711,-5.01668533600614));
#31867=CARTESIAN_POINT('Ctrl Pts',(-8.,-8.14527403028023,-5.21867499254995));
#31868=CARTESIAN_POINT('Ctrl Pts',(-8.,-8.01107409605472,-5.41905433262977));
#31869=CARTESIAN_POINT('Ctrl Pts',(-8.,-7.86944352784287,-5.61432559405275));
#31870=CARTESIAN_POINT('Ctrl Pts',(-8.,-7.72056574116336,-5.80400386624563));
#31871=CARTESIAN_POINT('Ctrl Pts',(-8.,-7.65750042133828,-5.8843524606633));
#31872=CARTESIAN_POINT('Ctrl Pts',(-8.,-7.59313416638248,-5.96369704112626));
#31873=CARTESIAN_POINT('Ctrl Pts',(-8.,-7.52747884839902,-6.0419988087639));
#31874=CARTESIAN_POINT('Ctrl Pts',(-8.,-7.42746572080017,-6.1612763466464));
#31875=CARTESIAN_POINT('Ctrl Pts',(-8.,-7.32446159078778,-6.27813441156677));
#31876=CARTESIAN_POINT('Ctrl Pts',(-8.,-7.21857424983126,-6.39248700007983));
#31877=CARTESIAN_POINT('Origin',(-8.,12.5,0.));
#31878=CARTESIAN_POINT('',(-8.,-12.5,-1.53080849893419E-15));
#31879=CARTESIAN_POINT('Origin',(-8.,0.,0.));
#31880=CARTESIAN_POINT('Origin',(-3.5,0.,0.));
#31881=CARTESIAN_POINT('Origin',(-4.,0.,0.));
#31882=CARTESIAN_POINT('',(0.,-12.5,-1.53080849893419E-15));
#31883=CARTESIAN_POINT('Origin',(0.,0.,0.));
#31884=CARTESIAN_POINT('',(-4.,-12.5,-1.53080849893419E-15));
#31885=CARTESIAN_POINT('Origin',(0.,13.5,0.));
#31886=CARTESIAN_POINT('',(0.,-13.5,-1.65327317884893E-15));
#31887=CARTESIAN_POINT('Origin',(0.,0.,0.));
#31888=CARTESIAN_POINT('Origin',(0.3,0.,0.));
#31889=CARTESIAN_POINT('',(0.6,-13.5,-1.65327317884893E-15));
#31890=CARTESIAN_POINT('Origin',(0.6,0.,0.));
#31891=CARTESIAN_POINT('',(0.3,-13.5,-1.65327317884893E-15));
#31892=CARTESIAN_POINT('Origin',(0.8,0.,0.));
#31893=CARTESIAN_POINT('',(1.,-13.1,-1.60428730688303E-15));
#31894=CARTESIAN_POINT('Origin',(1.,0.,0.));
#31895=CARTESIAN_POINT('',(0.8,-13.3,-1.62878024286598E-15));
#31896=CARTESIAN_POINT('Origin',(1.,9.6,0.));
#31897=CARTESIAN_POINT('',(0.,0.,0.));
#31898=CARTESIAN_POINT('Origin',(25.6,0.,0.));
#31899=CARTESIAN_POINT('',(22.9221761170896,-2.94337932284574,0.0024246877538029));
#31900=CARTESIAN_POINT('',(22.7778238829104,-2.94393084859299,0.00289653660730527));
#31901=CARTESIAN_POINT('',(25.6,-2.942,-3.60291088309151E-16));
#31902=CARTESIAN_POINT('',(22.6,1.28892185405323,2.64462557919718));
#31903=CARTESIAN_POINT('Ctrl Pts',(22.9221761170896,-2.94337932284574,0.0024246877538029));
#31904=CARTESIAN_POINT('Ctrl Pts',(22.912754340928,-2.9448569196983,0.17632691862541));
#31905=CARTESIAN_POINT('Ctrl Pts',(22.9033325647665,-2.93071733453316,0.349980573695374));
#31906=CARTESIAN_POINT('Ctrl Pts',(22.8939107886049,-2.90008429939073,0.520661013315647));
#31907=CARTESIAN_POINT('Ctrl Pts',(22.8419820569707,-2.73124833536721,1.46137734877704));
#31908=CARTESIAN_POINT('Ctrl Pts',(22.7900533253365,-2.06138509115311,2.31177528194959));
#31909=CARTESIAN_POINT('Ctrl Pts',(22.7381245937023,-1.186342977627,2.69686178609481));
#31910=CARTESIAN_POINT('Ctrl Pts',(22.6920830624682,-0.410505064140464,
3.0382907359358));
#31911=CARTESIAN_POINT('Ctrl Pts',(22.6460415312341,0.526626295037523,3.01393307256905));
#31912=CARTESIAN_POINT('Ctrl Pts',(22.6,1.291939685441,2.64724960214527));
#31913=CARTESIAN_POINT('',(22.6,-1.28892185405321,2.64462557919718));
#31914=CARTESIAN_POINT('Origin',(22.6,0.,0.));
#31915=CARTESIAN_POINT('Ctrl Pts',(22.6,-1.28892185405321,2.64462557919718));
#31916=CARTESIAN_POINT('Ctrl Pts',(22.6519287316342,-2.15180458522763,2.22407893605632));
#31917=CARTESIAN_POINT('Ctrl Pts',(22.7038574632684,-2.78633791211509,1.35244859465509));
#31918=CARTESIAN_POINT('Ctrl Pts',(22.7557861949026,-2.91785469712274,0.407185074986569));
#31919=CARTESIAN_POINT('Ctrl Pts',(22.7631320909052,-2.93645920747492,0.273467048529401));
#31920=CARTESIAN_POINT('Ctrl Pts',(22.7704779869078,-2.94499773028714,0.138275530460612));
#31921=CARTESIAN_POINT('Ctrl Pts',(22.7778238829104,-2.94393084859299,0.00289653660730527));
#31922=CARTESIAN_POINT('Origin',(25.6,0.,0.));
#31923=CARTESIAN_POINT('',(23.9221761170896,-2.9383190595815,-0.00138042702469643));
#31924=CARTESIAN_POINT('',(23.7778238829104,-2.93785684534219,-0.000854546637487877));
#31925=CARTESIAN_POINT('',(25.6,-2.942,-3.60291088309151E-16));
#31926=CARTESIAN_POINT('Ctrl Pts',(23.9221761170896,-2.9383190595815,-0.00138042702469643));
#31927=CARTESIAN_POINT('Ctrl Pts',(23.8909933973998,-2.93576543917648,0.576735544293962));
#31928=CARTESIAN_POINT('Ctrl Pts',(23.8598106777101,-2.77025503775714,1.15620073583879));
#31929=CARTESIAN_POINT('Ctrl Pts',(23.8286279580203,-2.45196769155219,1.63386091512667));
#31930=CARTESIAN_POINT('Ctrl Pts',(23.7766992263861,-1.92192225779668,2.42931068696698));
#31931=CARTESIAN_POINT('Ctrl Pts',(23.7247704947519,-0.968189696573736,
2.94243073120691));
#31932=CARTESIAN_POINT('Ctrl Pts',(23.6728417631178,-0.0123243431917003,
2.94643266533865));
#31933=CARTESIAN_POINT('Ctrl Pts',(23.6209130314836,0.943541010190328,2.95043459947038));
#31934=CARTESIAN_POINT('Ctrl Pts',(23.5689842998494,1.90153915573145,2.44531842349393));
#31935=CARTESIAN_POINT('Ctrl Pts',(23.5170555682152,2.43821811361518,1.65431992343549));
#31936=CARTESIAN_POINT('Ctrl Pts',(23.465126836581,2.97489707149892,0.863321423377055));
#31937=CARTESIAN_POINT('Ctrl Pts',(23.4131981049468,3.09025684172528,-0.213559400763362));
#31938=CARTESIAN_POINT('Ctrl Pts',(23.3612693733126,2.73332327778208,-1.10027216939385));
#31939=CARTESIAN_POINT('Ctrl Pts',(23.3093406416784,2.37638971383888,-1.98698493802435));
#31940=CARTESIAN_POINT('Ctrl Pts',(23.2574119100442,1.54716281572612,-2.68352965114492));
#31941=CARTESIAN_POINT('Ctrl Pts',(23.20548317841,0.612137108554167,-2.88214374660199));
#31942=CARTESIAN_POINT('Ctrl Pts',(23.1535544467758,-0.322888598617789,
-3.08075784205906));
#31943=CARTESIAN_POINT('Ctrl Pts',(23.1016257151416,-1.36371311484895,-2.78144131985263));
#31944=CARTESIAN_POINT('Ctrl Pts',(23.0496969835075,-2.05022103104806,-2.1162656898743));
#31945=CARTESIAN_POINT('Ctrl Pts',(23.0071900280348,-2.61217123678476,-1.57177731137621));
#31946=CARTESIAN_POINT('Ctrl Pts',(22.9646830725622,-2.93671304861665,-0.782146528701403));
#31947=CARTESIAN_POINT('Ctrl Pts',(22.9221761170896,-2.94337932284574,0.0024246877538029));
#31948=CARTESIAN_POINT('Ctrl Pts',(22.7778238829104,-2.94393084859299,0.00289653660730527));
#31949=CARTESIAN_POINT('Ctrl Pts',(22.822406718542,-2.93745585749709,-0.818729501766297));
#31950=CARTESIAN_POINT('Ctrl Pts',(22.8669895541736,-2.57717788935255,-1.64726097453814));
#31951=CARTESIAN_POINT('Ctrl Pts',(22.9115723898051,-1.96605887355123,-2.19521297425806));
#31952=CARTESIAN_POINT('Ctrl Pts',(22.9635011214393,-1.25424602184426,-2.83345080589834));
#31953=CARTESIAN_POINT('Ctrl Pts',(23.0154298530735,-0.202120075302478,
-3.09102977124308));
#31954=CARTESIAN_POINT('Ctrl Pts',(23.0673585847077,0.724516079376799,-2.85579333374966));
#31955=CARTESIAN_POINT('Ctrl Pts',(23.1192873163419,1.65115223405607,-2.62055689625624));
#31956=CARTESIAN_POINT('Ctrl Pts',(23.1712160479761,2.45229859687285,-1.89250505592465));
#31957=CARTESIAN_POINT('Ctrl Pts',(23.2231447796103,2.77422274277707,-0.992606024168016));
#31958=CARTESIAN_POINT('Ctrl Pts',(23.2750735112445,3.09614688868129,-0.0927069924113744));
#31959=CARTESIAN_POINT('Ctrl Pts',(23.3270022428787,2.93884881767296,0.979039230770322));
#31960=CARTESIAN_POINT('Ctrl Pts',(23.3789309745129,2.3716618413383,1.74848753980998));
#31961=CARTESIAN_POINT('Ctrl Pts',(23.430859706147,1.80447486500363,2.51793584884963));
#31962=CARTESIAN_POINT('Ctrl Pts',(23.4827884377812,0.827398983342636,2.98508624374724));
#31963=CARTESIAN_POINT('Ctrl Pts',(23.5347171694154,-0.127590825323999,
2.94366917333447));
#31964=CARTESIAN_POINT('Ctrl Pts',(23.5866459010496,-1.08258063399063,2.9022521029217));
#31965=CARTESIAN_POINT('Ctrl Pts',(23.6385746326838,-2.01548436966291,2.35226756719854));
#31966=CARTESIAN_POINT('Ctrl Pts',(23.690503364318,-2.5140002246829,1.53670433537425));
#31967=CARTESIAN_POINT('Ctrl Pts',(23.7196102038488,-2.79342590174055,1.07956880810663));
#31968=CARTESIAN_POINT('Ctrl Pts',(23.7487170433796,-2.93637680815486,0.538994508137228));
#31969=CARTESIAN_POINT('Ctrl Pts',(23.7778238829104,-2.93785684534219,-0.000854546637487877));
#31970=CARTESIAN_POINT('Origin',(25.6,0.,0.));
#31971=CARTESIAN_POINT('',(24.9221761170896,-2.94641400997859,0.000320893440124217));
#31972=CARTESIAN_POINT('',(24.7778238829104,-2.94641005469739,-0.000335482700479716));
#31973=CARTESIAN_POINT('',(25.6,-2.942,-3.60291088309151E-16));
#31974=CARTESIAN_POINT('Ctrl Pts',(24.9221761170896,-2.94641400997859,0.000320893440124217));
#31975=CARTESIAN_POINT('Ctrl Pts',(24.9211611855058,-2.94644390539513,0.0190039752988624));
#31976=CARTESIAN_POINT('Ctrl Pts',(24.9201462539221,-2.94628096860413,0.0376865226429225));
#31977=CARTESIAN_POINT('Ctrl Pts',(24.9191313223383,-2.94592358009294,0.0563653494972846));
#31978=CARTESIAN_POINT('Ctrl Pts',(24.8672025907041,-2.92763788243231,1.01206305610313));
#31979=CARTESIAN_POINT('Ctrl Pts',(24.8152738590699,-2.4003101053229,1.9580211429691));
#31980=CARTESIAN_POINT('Ctrl Pts',(24.7633451274357,-1.59702395175339,2.47611740807419));
#31981=CARTESIAN_POINT('Ctrl Pts',(24.7114163958015,-0.793737798183883,
2.99421367317928));
#31982=CARTESIAN_POINT('Ctrl Pts',(24.6594876641674,0.285506731845734,3.08444811652349));
#31983=CARTESIAN_POINT('Ctrl Pts',(24.6075589325332,1.16367382457068,2.70693656051822));
#31984=CARTESIAN_POINT('Ctrl Pts',(24.555630200899,2.04184091729562,2.32942500451294));
#31985=CARTESIAN_POINT('Ctrl Pts',(24.5037014692648,2.7189305727159,1.48416744915818));
#31986=CARTESIAN_POINT('Ctrl Pts',(24.4517727376306,2.8956628730315,0.544774888775652));
#31987=CARTESIAN_POINT('Ctrl Pts',(24.3998440059964,3.07239517334711,-0.394617671606881));
#31988=CARTESIAN_POINT('Ctrl Pts',(24.3479152743622,2.74877011855805,-1.42814523701718));
#31989=CARTESIAN_POINT('Ctrl Pts',(24.295986542728,2.06783319808421,-2.09897820914092));
#31990=CARTESIAN_POINT('Ctrl Pts',(24.2440578110938,1.38689627761036,-2.76981118126465));
#31991=CARTESIAN_POINT('Ctrl Pts',(24.1921290794596,0.348647491451722,-3.07794956010182));
#31992=CARTESIAN_POINT('Ctrl Pts',(24.1402003478254,-0.587998308823754,
-2.8871954022964));
#31993=CARTESIAN_POINT('Ctrl Pts',(24.0882716161913,-1.52464410909923,-2.69644124449098));
#31994=CARTESIAN_POINT('Ctrl Pts',(24.0363428845571,-2.35968692349154,-2.00679455004298));
#31995=CARTESIAN_POINT('Ctrl Pts',(23.9844141529229,-2.72402917754366,-1.12308145309864));
#31996=CARTESIAN_POINT('Ctrl Pts',(23.9636681409785,-2.86958730146767,-0.770029840095521));
#31997=CARTESIAN_POINT('Ctrl Pts',(23.942922129034,-2.94001799540079,-0.386003736523308));
#31998=CARTESIAN_POINT('Ctrl Pts',(23.9221761170896,-2.9383190595815,-0.00138042702469643));
#31999=CARTESIAN_POINT('Ctrl Pts',(23.7778238829104,-2.93785684534219,-0.000854546637487877));
#32000=CARTESIAN_POINT('Ctrl Pts',(23.8006457750138,-2.9390173027997,-0.42413570937398));
#32001=CARTESIAN_POINT('Ctrl Pts',(23.8234676671172,-2.85320560862381,-0.846971012582013));
#32002=CARTESIAN_POINT('Ctrl Pts',(23.8462895592206,-2.67801351714517,-1.22879127448483));
#32003=CARTESIAN_POINT('Ctrl Pts',(23.8982182908548,-2.27938298021973,-2.09758172459419));
#32004=CARTESIAN_POINT('Ctrl Pts',(23.950147022489,-1.41799393200115,-2.75402069688747));
#32005=CARTESIAN_POINT('Ctrl Pts',(24.0020757541231,-0.474601113597208,
-2.90798448590835));
#32006=CARTESIAN_POINT('Ctrl Pts',(24.0540044857573,0.468791704806728,-3.06194827492923));
#32007=CARTESIAN_POINT('Ctrl Pts',(24.1059332173915,1.49418829339602,-2.71343688067772));
#32008=CARTESIAN_POINT('Ctrl Pts',(24.1578619490257,2.14836063534518,-2.0164811236668));
#32009=CARTESIAN_POINT('Ctrl Pts',(24.2097906806599,2.80253297729433,-1.31952536665587));
#32010=CARTESIAN_POINT('Ctrl Pts',(24.2617194122941,3.08548107260335,-0.274125246885542));
#32011=CARTESIAN_POINT('Ctrl Pts',(24.3136481439283,2.87213594284245,0.657635574862683));
#32012=CARTESIAN_POINT('Ctrl Pts',(24.3655768755625,2.65879081308155,1.58939639661091));
#32013=CARTESIAN_POINT('Ctrl Pts',(24.4175056071966,1.94915245825073,2.40751792033702));
#32014=CARTESIAN_POINT('Ctrl Pts',(24.4694343388308,1.05688918030864,2.75038672001481));
#32015=CARTESIAN_POINT('Ctrl Pts',(24.521363070465,0.164625902366541,3.0932555196926));
#32016=CARTESIAN_POINT('Ctrl Pts',(24.5732918020992,-0.910262298686838,
2.96087159532206));
#32017=CARTESIAN_POINT('Ctrl Pts',(24.6252205337334,-1.69266594113809,2.41174795315879));
#32018=CARTESIAN_POINT('Ctrl Pts',(24.6760883167924,-2.45908440537369,1.87384337850255));
#32019=CARTESIAN_POINT('Ctrl Pts',(24.7269560998514,-2.94484764344756,0.936053831091904));
#32020=CARTESIAN_POINT('Ctrl Pts',(24.7778238829104,-2.94641005469739,-0.000335482700479716));
#32021=CARTESIAN_POINT('Origin',(25.6,0.,0.));
#32022=CARTESIAN_POINT('',(25.9221761170896,-2.93786869100257,0.000876386695073395));
#32023=CARTESIAN_POINT('',(25.7778238829104,-2.93833233985647,0.00139222834412371));
#32024=CARTESIAN_POINT('',(25.6,-2.942,-3.60291088309151E-16));
#32025=CARTESIAN_POINT('Ctrl Pts',(25.9221761170896,-2.93786869100257,0.000876386695073395));
#32026=CARTESIAN_POINT('Ctrl Pts',(25.8994002419776,-2.93904020397999,0.423294701449549));
#32027=CARTESIAN_POINT('Ctrl Pts',(25.8766243668657,-2.85358407529444,0.845261266561695));
#32028=CARTESIAN_POINT('Ctrl Pts',(25.8538484917537,-2.67907431130908,1.22645975976682));
#32029=CARTESIAN_POINT('Ctrl Pts',(25.8019197601195,-2.28119406929874,2.09558791206413));
#32030=CARTESIAN_POINT('Ctrl Pts',(25.7499910284854,-1.42038210979013,2.75278947109579));
#32031=CARTESIAN_POINT('Ctrl Pts',(25.6980622968512,-0.477125112358299,
2.90757535073352));
#32032=CARTESIAN_POINT('Ctrl Pts',(25.646133565217,0.466131885073529,3.06236123037125));
#32033=CARTESIAN_POINT('Ctrl Pts',(25.5942048335828,1.49183392042857,2.71473143061506));
#32034=CARTESIAN_POINT('Ctrl Pts',(25.5422761019486,2.14661136587812,2.01834149796711));
#32035=CARTESIAN_POINT('Ctrl Pts',(25.4903473703144,2.80138881132767,1.32195156531916));
#32036=CARTESIAN_POINT('Ctrl Pts',(25.4384186386802,3.08524166687174,0.276801499779447));
#32037=CARTESIAN_POINT('Ctrl Pts',(25.386489907046,2.87270439640652,-0.655142892352426));
#32038=CARTESIAN_POINT('Ctrl Pts',(25.3345611754118,2.6601671259413,-1.5870872844843));
#32039=CARTESIAN_POINT('Ctrl Pts',(25.2826324437776,1.95123972946679,-2.40582600320835));
#32040=CARTESIAN_POINT('Ctrl Pts',(25.2307037121434,1.05927455670128,-2.74946907721497));
#32041=CARTESIAN_POINT('Ctrl Pts',(25.1787749805093,0.16730938393577,-3.0931121512216));
#32042=CARTESIAN_POINT('Ctrl Pts',(25.1268462488751,-0.907693565120746,
-2.9616595805108));
#32043=CARTESIAN_POINT('Ctrl Pts',(25.0749175172409,-1.69057323054308,-2.41321463198254));
#32044=CARTESIAN_POINT('Ctrl Pts',(25.0240037171904,-2.45815174622199,-1.87548887652329));
#32045=CARTESIAN_POINT('Ctrl Pts',(24.97308991714,-2.94491431356086,-0.936911437587762));
#32046=CARTESIAN_POINT('Ctrl Pts',(24.9221761170896,-2.94641400997859,0.000320893440124217));
#32047=CARTESIAN_POINT('Ctrl Pts',(24.7778238829104,-2.94641005469739,-0.000335482700479716));
#32048=CARTESIAN_POINT('Ctrl Pts',(24.7788848314856,-2.94644264188499,-0.0198657403321496));
#32049=CARTESIAN_POINT('Ctrl Pts',(24.7799457800608,-2.94626459502485,-0.0393953888428549));
#32050=CARTESIAN_POINT('Ctrl Pts',(24.781006728636,-2.94587406733219,-0.0589207873412386));
#32051=CARTESIAN_POINT('Ctrl Pts',(24.8329354602702,-2.92675946722594,-1.01460252572203));
#32052=CARTESIAN_POINT('Ctrl Pts',(24.8848641919044,-2.3986111831643,-1.96010264252762));
#32053=CARTESIAN_POINT('Ctrl Pts',(24.9367929235386,-1.59487577768028,-2.47750198725934));
#32054=CARTESIAN_POINT('Ctrl Pts',(24.9887216551728,-0.791140372196265,
-2.99490133199106));
#32055=CARTESIAN_POINT('Ctrl Pts',(25.0406503868069,0.288182154710141,-3.08419990464891));
#32056=CARTESIAN_POINT('Ctrl Pts',(25.0925791184411,1.16602155650292,-2.70592667620281));
#32057=CARTESIAN_POINT('Ctrl Pts',(25.1445078500753,2.0438609582957,-2.32765344775672));
#32058=CARTESIAN_POINT('Ctrl Pts',(25.1964365817095,2.72021723497484,-1.48180841820668));
#32059=CARTESIAN_POINT('Ctrl Pts',(25.2483653133437,2.89613471145009,-0.54226290020962));
#32060=CARTESIAN_POINT('Ctrl Pts',(25.3002940449779,3.07205218792534,0.39728261778744));
#32061=CARTESIAN_POINT('Ctrl Pts',(25.3522227766121,2.74753086419669,1.43052862423153));
#32062=CARTESIAN_POINT('Ctrl Pts',(25.4041515082463,2.06601214166399,2.1007710646963));
#32063=CARTESIAN_POINT('Ctrl Pts',(25.4560802398804,1.38449341913129,2.77101350516106));
#32064=CARTESIAN_POINT('Ctrl Pts',(25.5080089715146,0.345977297794549,3.07825237964651));
#32065=CARTESIAN_POINT('Ctrl Pts',(25.5599377031488,-0.590502677571841,
2.8866852803957));
#32066=CARTESIAN_POINT('Ctrl Pts',(25.611866434783,-1.52698265293823,2.69511818114489));
#32067=CARTESIAN_POINT('Ctrl Pts',(25.6637951664172,-2.36142648233428,2.00474510815782));
#32068=CARTESIAN_POINT('Ctrl Pts',(25.7157238980514,-2.72500240918793,1.12071725070303));
#32069=CARTESIAN_POINT('Ctrl Pts',(25.7364238930044,-2.86993219302934,0.768323275118707));
#32070=CARTESIAN_POINT('Ctrl Pts',(25.7571238879574,-2.94004086870962,0.38515747266671));
#32071=CARTESIAN_POINT('Ctrl Pts',(25.7778238829104,-2.93833233985647,0.00139222834412371));
#32072=CARTESIAN_POINT('Origin',(25.6,0.,0.));
#32073=CARTESIAN_POINT('',(26.9221761170896,-2.94442477429212,-0.00197218427072376));
#32074=CARTESIAN_POINT('',(26.7778238829104,-2.94339904745569,-0.00227025699168395));
#32075=CARTESIAN_POINT('',(25.6,-2.942,-3.60291088309151E-16));
#32076=CARTESIAN_POINT('Ctrl Pts',(26.9221761170896,-2.94442477429212,-0.00197218427072376));
#32077=CARTESIAN_POINT('Ctrl Pts',(26.8776392984494,-2.93802580261633,0.819340609163623));
#32078=CARTESIAN_POINT('Ctrl Pts',(26.8331024798093,-2.57794208161663,1.6455819227055));
#32079=CARTESIAN_POINT('Ctrl Pts',(26.7885656611692,-1.96775235997052,2.19307773506812));
#32080=CARTESIAN_POINT('Ctrl Pts',(26.736636929535,-1.25628757041458,2.831443114076));
#32081=CARTESIAN_POINT('Ctrl Pts',(26.6847081979008,-0.204805367471877,
3.09085587275804));
#32082=CARTESIAN_POINT('Ctrl Pts',(26.6327794662666,0.721931053663677,2.85665174834169));
#32083=CARTESIAN_POINT('Ctrl Pts',(26.5808507346324,1.64866747479923,2.62244762392534));
#32084=CARTESIAN_POINT('Ctrl Pts',(26.5289220029982,2.45065811412763,1.89462661641059));
#32085=CARTESIAN_POINT('Ctrl Pts',(26.476993271364,2.77341506728714,0.99489296823238));
#32086=CARTESIAN_POINT('Ctrl Pts',(26.4250645397298,3.09617202044665,0.0951593200541696));
#32087=CARTESIAN_POINT('Ctrl Pts',(26.3731358080956,2.93969528743728,-0.976486968787502));
#32088=CARTESIAN_POINT('Ctrl Pts',(26.3212070764614,2.37314939075441,-1.7463688848073));
#32089=CARTESIAN_POINT('Ctrl Pts',(26.2692783448273,1.80660349407155,-2.5162508008271));
#32090=CARTESIAN_POINT('Ctrl Pts',(26.2173496131931,0.829988433715184,-2.98436834402501));
#32091=CARTESIAN_POINT('Ctrl Pts',(26.1654208815589,-0.125023259080066,
-2.94380911502955));
#32092=CARTESIAN_POINT('Ctrl Pts',(26.1134921499247,-1.08003495187532,-2.90324988603409));
#32093=CARTESIAN_POINT('Ctrl Pts',(26.0615634182905,-2.01344327710945,-2.35401388484526));
#32094=CARTESIAN_POINT('Ctrl Pts',(26.0096346866563,-2.51267317747048,-1.53886851146936));
#32095=CARTESIAN_POINT('Ctrl Pts',(25.9804818301341,-2.79294148364365,-1.08124485368015));
#32096=CARTESIAN_POINT('Ctrl Pts',(25.9513289736118,-2.93636916795125,-0.539814166878388));
#32097=CARTESIAN_POINT('Ctrl Pts',(25.9221761170896,-2.93786869100257,0.000876386695073395));
#32098=CARTESIAN_POINT('Ctrl Pts',(25.7778238829104,-2.93833233985647,0.00139222834412371));
#32099=CARTESIAN_POINT('Ctrl Pts',(25.8090526195916,-2.93575479344698,-0.577569447229037));
#32100=CARTESIAN_POINT('Ctrl Pts',(25.8402813562728,-2.76972275937453,-1.15789544023111));
#32101=CARTESIAN_POINT('Ctrl Pts',(25.871510092954,-2.45055050830498,-1.6359851748563));
#32102=CARTESIAN_POINT('Ctrl Pts',(25.9234388245882,-1.91981465625711,-2.43097710103833));
#32103=CARTESIAN_POINT('Ctrl Pts',(25.9753675562224,-0.965634927850109,
-2.9432783114799));
#32104=CARTESIAN_POINT('Ctrl Pts',(26.0272962878566,-0.00976743849944818,
-2.94644699891546));
#32105=CARTESIAN_POINT('Ctrl Pts',(26.0792250194907,0.946100050851219,-2.94961568635102));
#32106=CARTESIAN_POINT('Ctrl Pts',(26.1311537511249,1.90365530114555,-2.44365185078057));
#32107=CARTESIAN_POINT('Ctrl Pts',(26.1830824827591,2.43965021452719,-1.65219613439981));
#32108=CARTESIAN_POINT('Ctrl Pts',(26.2350112143933,2.97564512790882,-0.860740418019046));
#32109=CARTESIAN_POINT('Ctrl Pts',(26.2869399460275,3.09007970437777,0.216207179172027));
#32110=CARTESIAN_POINT('Ctrl Pts',(26.3388686776617,2.73237278071044,1.10262609575619));
#32111=CARTESIAN_POINT('Ctrl Pts',(26.3907974092959,2.37466585704312,1.98904501234035));
#32112=CARTESIAN_POINT('Ctrl Pts',(26.4427261409301,1.54481743323954,2.6849352483176));
#32113=CARTESIAN_POINT('Ctrl Pts',(26.4946548725643,0.609628131457622,2.88270688564602));
#32114=CARTESIAN_POINT('Ctrl Pts',(26.5465836041984,-0.325561170324308,
3.08047852297444));
#32115=CARTESIAN_POINT('Ctrl Pts',(26.5985123358326,-1.36609135008459,2.780131561654));
#32116=CARTESIAN_POINT('Ctrl Pts',(26.6504410674668,-2.05203877789913,2.11442230812662));
#32117=CARTESIAN_POINT('Ctrl Pts',(26.692902005948,-2.61292233151529,1.57008704764869));
#32118=CARTESIAN_POINT('Ctrl Pts',(26.7353629444292,-2.93673328995051,0.78147203492828));
#32119=CARTESIAN_POINT('Ctrl Pts',(26.7778238829104,-2.94339904745569,-0.00227025699168395));
#32120=CARTESIAN_POINT('Origin',(25.6,0.,0.));
#32121=CARTESIAN_POINT('',(27.9221761170896,-2.94084529159276,0.00236346891266642));
#32122=CARTESIAN_POINT('',(27.7778238829104,-2.9419205159921,0.00243417433800859));
#32123=CARTESIAN_POINT('',(25.6,-2.942,-3.60291088309151E-16));
#32124=CARTESIAN_POINT('Ctrl Pts',(27.9221761170896,-2.94084529159276,0.00236346891266642));
#32125=CARTESIAN_POINT('Ctrl Pts',(27.9078070865555,-2.94302846982566,0.268201177356569));
#32126=CARTESIAN_POINT('Ctrl Pts',(27.8934380560213,-2.90984722496843,0.533507849845637));
#32127=CARTESIAN_POINT('Ctrl Pts',(27.8790690254872,-2.83909368778622,0.788374135968067));
#32128=CARTESIAN_POINT('Ctrl Pts',(27.827140293853,-2.5833950562207,1.70944413739935));
#32129=CARTESIAN_POINT('Ctrl Pts',(27.7752115622188,-1.83698271972066,2.49415725566241));
#32130=CARTESIAN_POINT('Ctrl Pts',(27.7232828305846,-0.929946677882633,
2.79582967865374));
#32131=CARTESIAN_POINT('Ctrl Pts',(27.6713540989504,-0.0229106360446091,
3.09750210164506));
#32132=CARTESIAN_POINT('Ctrl Pts',(27.6194253673162,1.0447491111314,2.91613382936466));
#32133=CARTESIAN_POINT('Ctrl Pts',(27.567496635682,1.80120320149326,2.33180659887102));
#32134=CARTESIAN_POINT('Ctrl Pts',(27.5155679040478,2.55765729185511,1.74747936837739));
#32135=CARTESIAN_POINT('Ctrl Pts',(27.4636391724136,3.00290572540282,0.760193179670536));
#32136=CARTESIAN_POINT('Ctrl Pts',(27.4117104407794,2.94010093297105,-0.193619427174991));
#32137=CARTESIAN_POINT('Ctrl Pts',(27.3597817091452,2.87729614053928,-1.14743203402053));
#32138=CARTESIAN_POINT('Ctrl Pts',(27.3078529775111,2.30643812212801,-2.06777105900474));
#32139=CARTESIAN_POINT('Ctrl Pts',(27.2559242458769,1.47987354517457,-2.54786020635006));
#32140=CARTESIAN_POINT('Ctrl Pts',(27.2039955142427,0.653308968221138,-3.02794935369537));
#32141=CARTESIAN_POINT('Ctrl Pts',(27.1520667826085,-0.428962167274455,
-3.0677886234018));
#32142=CARTESIAN_POINT('Ctrl Pts',(27.1001380509743,-1.28857750153804,-2.64975754983817));
#32143=CARTESIAN_POINT('Ctrl Pts',(27.0482093193401,-2.14819283580162,-2.23172647627454));
#32144=CARTESIAN_POINT('Ctrl Pts',(26.9962805877059,-2.7851523688332,-1.35582505944085));
#32145=CARTESIAN_POINT('Ctrl Pts',(26.9443518560717,-2.91790844726441,-0.409215351357154));
#32146=CARTESIAN_POINT('Ctrl Pts',(26.9369599430777,-2.93680591212272,-0.274468047094759));
#32147=CARTESIAN_POINT('Ctrl Pts',(26.9295680300836,-2.94548683133442,-0.138287998810961));
#32148=CARTESIAN_POINT('Ctrl Pts',(26.9221761170896,-2.94442477429212,-0.00197218427072376));
#32149=CARTESIAN_POINT('Ctrl Pts',(26.7778238829104,-2.94339904745569,-0.00227025699168395));
#32150=CARTESIAN_POINT('Ctrl Pts',(26.7872916760634,-2.94488535500151,-0.177026401593688));
#32151=CARTESIAN_POINT('Ctrl Pts',(26.7967594692164,-2.93060366699902,-0.351540281644112));
#32152=CARTESIAN_POINT('Ctrl Pts',(26.8062272623694,-2.89966629313921,-0.523049776019018));
#32153=CARTESIAN_POINT('Ctrl Pts',(26.8581559940036,-2.72998170469592,-1.46374106090295));
#32154=CARTESIAN_POINT('Ctrl Pts',(26.9100847256378,-2.05924785194055,-2.31405208493648));
#32155=CARTESIAN_POINT('Ctrl Pts',(26.962013457272,-1.18393581131734,-2.69813679648287));
#32156=CARTESIAN_POINT('Ctrl Pts',(27.0139421889062,-0.308623770694144,
-3.08222150802926));
#32157=CARTESIAN_POINT('Ctrl Pts',(27.0658709205403,0.77126645779688,-3.00007990708851));
#32158=CARTESIAN_POINT('Ctrl Pts',(27.1177996521745,1.57841480666123,-2.48802101020065));
#32159=CARTESIAN_POINT('Ctrl Pts',(27.1697283838087,2.38556315552559,-1.9759621133128));
#32160=CARTESIAN_POINT('Ctrl Pts',(27.2216571154429,2.91996962476327,-1.03398592047784));
#32161=CARTESIAN_POINT('Ctrl Pts',(27.2735858470771,2.9454192977785,-0.0784511552908093));
#32162=CARTESIAN_POINT('Ctrl Pts',(27.3255145787113,2.97086897079373,0.87708360989624));
#32163=CARTESIAN_POINT('Ctrl Pts',(27.3774433103455,2.48736184758648,1.84617694743536));
#32164=CARTESIAN_POINT('Ctrl Pts',(27.4293720419797,1.7086171945732,2.40047429147118));
#32165=CARTESIAN_POINT('Ctrl Pts',(27.4813007736139,0.929872541559935,2.95477163550698));
#32166=CARTESIAN_POINT('Ctrl Pts',(27.5332295052481,-0.144109641259354,
3.09427298603949));
#32167=CARTESIAN_POINT('Ctrl Pts',(27.5851582368823,-1.03862876920953,2.75733027892591));
#32168=CARTESIAN_POINT('Ctrl Pts',(27.6370869685165,-1.93314789715972,2.42038757181232));
#32169=CARTESIAN_POINT('Ctrl Pts',(27.6890157001506,-2.6482039702408,1.60700080705263));
#32170=CARTESIAN_POINT('Ctrl Pts',(27.7409444317848,-2.86771742957133,0.676669149876849));
#32171=CARTESIAN_POINT('Ctrl Pts',(27.75323758216,-2.91968311176705,0.456430630649596));
#32172=CARTESIAN_POINT('Ctrl Pts',(27.7655307325352,-2.94387776538163,0.229638326017039));
#32173=CARTESIAN_POINT('Ctrl Pts',(27.7778238829104,-2.9419205159921,0.00243417433800859));
#32174=CARTESIAN_POINT('Origin',(20.751410108095,0.,0.));
#32175=CARTESIAN_POINT('',(28.251410108095,-2.37081910956327,0.00190535601414123));
#32176=CARTESIAN_POINT('',(28.448589891905,-2.36902607076732,-0.00230475997383739));
#32177=CARTESIAN_POINT('',(20.751410108095,-2.37175,-2.19152050672682E-14));
#32178=CARTESIAN_POINT('',(28.658,1.97801633036407,-1.31405326343373));
#32179=CARTESIAN_POINT('Ctrl Pts',(28.251410108095,-2.37081910956327,0.00190535601414134));
#32180=CARTESIAN_POINT('Ctrl Pts',(28.288969809195,-2.36621855598052,-0.558287395810164));
#32181=CARTESIAN_POINT('Ctrl Pts',(28.3784582419293,-1.89114103981992,-1.89995231291283));
#32182=CARTESIAN_POINT('Ctrl Pts',(28.5139882058976,0.229773146349892,-2.73041805462421));
#32183=CARTESIAN_POINT('Ctrl Pts',(28.6119584687659,1.59534824541231,-1.88115502388143));
#32184=CARTESIAN_POINT('Ctrl Pts',(28.658,1.97801633036407,-1.31405326343373));
#32185=CARTESIAN_POINT('',(28.658,-0.598340649004819,-2.29503519150546));
#32186=CARTESIAN_POINT('Origin',(28.658,0.,0.));
#32187=CARTESIAN_POINT('Ctrl Pts',(28.448589891905,-2.36902607076732,-0.00230475997383763));
#32188=CARTESIAN_POINT('Ctrl Pts',(28.4664645296358,-2.37066543904879,-0.26930526887278));
#32189=CARTESIAN_POINT('Ctrl Pts',(28.5362678990008,-2.20751399255987,-1.30936831204417));
#32190=CARTESIAN_POINT('Ctrl Pts',(28.6060712683658,-1.34715978233134,-2.09980989479535));
#32191=CARTESIAN_POINT('Ctrl Pts',(28.658,-0.598340649004787,-2.29503519150547));
#32192=CARTESIAN_POINT('Origin',(20.751410108095,0.,0.));
#32193=CARTESIAN_POINT('',(27.251410108095,-2.3737047785273,-0.00158991435897493));
#32194=CARTESIAN_POINT('',(27.448589891905,-2.37168592243517,0.00196235655545912));
#32195=CARTESIAN_POINT('',(20.751410108095,-2.37175,-2.19152050672682E-14));
#32196=CARTESIAN_POINT('Ctrl Pts',(27.251410108095,-2.3737047785273,-0.00158991435897499));
#32197=CARTESIAN_POINT('Ctrl Pts',(27.258802021089,-2.37456097628056,-0.111483535411255));
#32198=CARTESIAN_POINT('Ctrl Pts',(27.3181226657173,-2.31839918246699,-0.992509565802802));
#32199=CARTESIAN_POINT('Ctrl Pts',(27.4293720419797,-1.21830985242857,-2.50527411810993));
#32200=CARTESIAN_POINT('Ctrl Pts',(27.5851582368822,1.39917134975873,-2.40892253286906));
#32201=CARTESIAN_POINT('Ctrl Pts',(27.7409444317848,2.77979593014647,-0.183075405908203));
#32202=CARTESIAN_POINT('Ctrl Pts',(27.8967306266874,1.70295911274323,2.20468395989619));
#32203=CARTESIAN_POINT('Ctrl Pts',(28.05251682159,-0.879184332564077,2.64332454430922));
#32204=CARTESIAN_POINT('Ctrl Pts',(28.1707433153925,-2.24915776353418,1.20305343625789));
#32205=CARTESIAN_POINT('Ctrl Pts',(28.2370410775608,-2.37257912077125,0.216215548060989));
#32206=CARTESIAN_POINT('Ctrl Pts',(28.251410108095,-2.37081910956327,0.00190535601414134));
#32207=CARTESIAN_POINT('Ctrl Pts',(27.448589891905,-2.37168592243517,0.00196235655545921));
#32208=CARTESIAN_POINT('Ctrl Pts',(27.488225473164,-2.36659853931644,-0.588598341501691));
#32209=CARTESIAN_POINT('Ctrl Pts',(27.5797897860572,-1.84853809447402,-1.9608582117688));
#32210=CARTESIAN_POINT('Ctrl Pts',(27.7232828305846,0.430422244683163,-2.75224826615359));
#32211=CARTESIAN_POINT('Ctrl Pts',(27.8790690254871,2.52434834774427,-1.17871200290743));
#32212=CARTESIAN_POINT('Ctrl Pts',(28.0348552203897,2.38625876548845,1.43744121743837));
#32213=CARTESIAN_POINT('Ctrl Pts',(28.1906414152923,0.139550436043699,2.78166084946855));
#32214=CARTESIAN_POINT('Ctrl Pts',(28.328552972464,-1.96011683010446,1.79687640253636));
#32215=CARTESIAN_POINT('Ctrl Pts',(28.4145357980016,-2.36590280739046,0.506374662749581));
#32216=CARTESIAN_POINT('Ctrl Pts',(28.448589891905,-2.36902607076732,-0.00230475997383763));
#32217=CARTESIAN_POINT('Origin',(20.751410108095,0.,0.));
#32218=CARTESIAN_POINT('',(26.251410108095,-2.36841946563064,0.00070651602448273));
#32219=CARTESIAN_POINT('',(26.448589891905,-2.37287786906969,-0.00183021142759643));
#32220=CARTESIAN_POINT('',(20.751410108095,-2.37175,-2.19152050672682E-14));
#32221=CARTESIAN_POINT('Ctrl Pts',(26.251410108095,-2.36841946563064,0.000706516024482698));
#32222=CARTESIAN_POINT('Ctrl Pts',(26.2805629646172,-2.36721059622311,-0.435181594253511));
#32223=CARTESIAN_POINT('Ctrl Pts',(26.3616445527737,-2.04562220805805,-1.64915798041796));
#32224=CARTESIAN_POINT('Ctrl Pts',(26.4946548725642,-0.118205880943649,
-2.78328803637694));
#32225=CARTESIAN_POINT('Ctrl Pts',(26.6504410674669,2.24374527752018,-1.65114209849832));
#32226=CARTESIAN_POINT('Ctrl Pts',(26.8062272623694,2.62218547960889,0.940642828993458));
#32227=CARTESIAN_POINT('Ctrl Pts',(26.962013457272,0.682564848581893,2.70088362563495));
#32228=CARTESIAN_POINT('Ctrl Pts',(27.1104077391805,-1.73978919606127,2.10326100923035));
#32229=CARTESIAN_POINT('Ctrl Pts',(27.2068732894548,-2.36854612418603,0.660527222904082));
#32230=CARTESIAN_POINT('Ctrl Pts',(27.251410108095,-2.3737047785273,-0.00158991435897499));
#32231=CARTESIAN_POINT('Ctrl Pts',(26.448589891905,-2.37287786906969,-0.00183021142759631));
#32232=CARTESIAN_POINT('Ctrl Pts',(26.458057685058,-2.37407608454277,-0.142713245404422));
#32233=CARTESIAN_POINT('Ctrl Pts',(26.5194542098452,-2.29941387975957,-1.05504174939956));
#32234=CARTESIAN_POINT('Ctrl Pts',(26.6327794662666,-1.11937732072311,-2.55101230581224));
#32235=CARTESIAN_POINT('Ctrl Pts',(26.7885656611692,1.49234563926014,-2.35235220176952));
#32236=CARTESIAN_POINT('Ctrl Pts',(26.9443518560717,2.78481186300027,-0.0741754152063169));
#32237=CARTESIAN_POINT('Ctrl Pts',(27.1001380509743,1.61544610555625,2.26958439782059));
#32238=CARTESIAN_POINT('Ctrl Pts',(27.2559242458769,-0.981988199781967,
2.60696950467868));
#32239=CARTESIAN_POINT('Ctrl Pts',(27.3720748595205,-2.27136583806211,1.14028354082802));
#32240=CARTESIAN_POINT('Ctrl Pts',(27.4362967415298,-2.37326379675183,0.185127362247078));
#32241=CARTESIAN_POINT('Ctrl Pts',(27.448589891905,-2.37168592243517,0.00196235655545921));
#32242=CARTESIAN_POINT('Origin',(20.751410108095,0.,0.));
#32243=CARTESIAN_POINT('',(25.251410108095,-2.3753084392137,0.000258694431195401));
#32244=CARTESIAN_POINT('',(25.448589891905,-2.36879324508993,0.00112237171147556));
#32245=CARTESIAN_POINT('',(20.751410108095,-2.37175,-2.19152050672682E-14));
#32246=CARTESIAN_POINT('Ctrl Pts',(25.251410108095,-2.3753084392137,0.000258694431195337));
#32247=CARTESIAN_POINT('Ctrl Pts',(25.3023239081454,-2.37409943004349,-0.755309212134195));
#32248=CARTESIAN_POINT('Ctrl Pts',(25.40516643983,-1.58145089662375,-2.28369713756637));
#32249=CARTESIAN_POINT('Ctrl Pts',(25.5599377031489,1.00151402983497,-2.59954499634369));
#32250=CARTESIAN_POINT('Ctrl Pts',(25.7157238980514,2.71606048046896,-0.619419004365017));
#32251=CARTESIAN_POINT('Ctrl Pts',(25.871510092954,2.02956013022766,1.90828459992846));
#32252=CARTESIAN_POINT('Ctrl Pts',(26.0272962878565,-0.451108261023179,
2.74902998834288));
#32253=CARTESIAN_POINT('Ctrl Pts',(26.1539296262369,-2.14339859605789,1.45702209482582));
#32254=CARTESIAN_POINT('Ctrl Pts',(26.228634232983,-2.36936390339549,0.341247181564567));
#32255=CARTESIAN_POINT('Ctrl Pts',(26.251410108095,-2.36841946563064,0.000706516024482698));
#32256=CARTESIAN_POINT('Ctrl Pts',(25.448589891905,-2.36879324508993,0.00112237171147545));
#32257=CARTESIAN_POINT('Ctrl Pts',(25.4798186285862,-2.36671530637589,-0.465618741150741));
#32258=CARTESIAN_POINT('Ctrl Pts',(25.5629760969016,-2.01029292083154,-1.71140950661792));
#32259=CARTESIAN_POINT('Ctrl Pts',(25.6980622968511,-0.00923482980258066,
-2.78578202961156));
#32260=CARTESIAN_POINT('Ctrl Pts',(25.8538484917537,2.30662002902024,-1.5621045377548));
#32261=CARTESIAN_POINT('Ctrl Pts',(26.0096346866563,2.58338094683827,1.04250164542461));
#32262=CARTESIAN_POINT('Ctrl Pts',(26.1654208815589,0.576386046271133,2.72551762147395));
#32263=CARTESIAN_POINT('Ctrl Pts',(26.3117392833084,-1.7872040174662,2.04327206314306));
#32264=CARTESIAN_POINT('Ctrl Pts',(26.4061289534238,-2.36750414019038,0.629998741958249));
#32265=CARTESIAN_POINT('Ctrl Pts',(26.448589891905,-2.37287786906969,-0.00183021142759631));
#32266=CARTESIAN_POINT('Origin',(20.751410108095,0.,0.));
#32267=CARTESIAN_POINT('',(24.251410108095,-2.36878253894032,-0.00111285785031767));
#32268=CARTESIAN_POINT('',(24.448589891905,-2.37530525058753,-0.000270455844553485));
#32269=CARTESIAN_POINT('',(20.751410108095,-2.37175,-2.19152050672682E-14));
#32270=CARTESIAN_POINT('Ctrl Pts',(24.251410108095,-2.36878253894032,-0.00111285785031799));
#32271=CARTESIAN_POINT('Ctrl Pts',(24.2721561200394,-2.37015216879397,-0.311184351495253));
#32272=CARTESIAN_POINT('Ctrl Pts',(24.344830863618,-2.17125111101719,-1.39570012081226));
#32273=CARTESIAN_POINT('Ctrl Pts',(24.4694343388309,-0.555935374140417,
-2.72976005070651));
#32274=CARTESIAN_POINT('Ctrl Pts',(24.6252205337334,1.95507743201704,-1.9845249725212));
#32275=CARTESIAN_POINT('Ctrl Pts',(24.781006728636,2.73776715706389,0.51506952434679));
#32276=CARTESIAN_POINT('Ctrl Pts',(24.9367929235385,1.10022053207099,2.55933153003611));
#32277=CARTESIAN_POINT('Ctrl Pts',(25.0925791184411,-1.50994080113541,2.3410988233723));
#32278=CARTESIAN_POINT('Ctrl Pts',(25.1974515132933,-2.36848045691257,0.800989302251748));
#32279=CARTESIAN_POINT('Ctrl Pts',(25.2503951765112,-2.37533253997991,0.0153204209432519));
#32280=CARTESIAN_POINT('Ctrl Pts',(25.251410108095,-2.3753084392137,0.000258694431195337));
#32281=CARTESIAN_POINT('Ctrl Pts',(24.448589891905,-2.37530525058753,-0.000270455844553585));
#32282=CARTESIAN_POINT('Ctrl Pts',(24.4496508404802,-2.37533152137686,-0.0160151494332644));
#32283=CARTESIAN_POINT('Ctrl Pts',(24.5026405206896,-2.36816253880158,-0.802368302582885));
#32284=CARTESIAN_POINT('Ctrl Pts',(24.6075589325332,-1.50790971480175,-2.34240766296688));
#32285=CARTESIAN_POINT('Ctrl Pts',(24.7633451274357,1.10244025446093,-2.55837695905924));
#32286=CARTESIAN_POINT('Ctrl Pts',(24.9191313223383,2.738213197235,-0.512694142435889));
#32287=CARTESIAN_POINT('Ctrl Pts',(25.0749175172409,1.95335583875086,1.98621940187114));
#32288=CARTESIAN_POINT('Ctrl Pts',(25.2307037121435,-0.558303519624818,
2.72927902174966));
#32289=CARTESIAN_POINT('Ctrl Pts',(25.3552611703648,-2.1718644533066,1.39430717464036));
#32290=CARTESIAN_POINT('Ctrl Pts',(25.427889896952,-2.3701706085527,0.310502119577585));
#32291=CARTESIAN_POINT('Ctrl Pts',(25.448589891905,-2.36879324508993,0.00112237171147545));
#32292=CARTESIAN_POINT('Origin',(20.751410108095,0.,0.));
#32293=CARTESIAN_POINT('',(23.251410108095,-2.37286196769524,0.00195470876282933));
#32294=CARTESIAN_POINT('',(23.448589891905,-2.36840991602323,-0.000688909241090413));
#32295=CARTESIAN_POINT('',(20.751410108095,-2.37175,-2.19152050672682E-14));
#32296=CARTESIAN_POINT('Ctrl Pts',(23.251410108095,-2.37286196769524,0.00195470876282933));
#32297=CARTESIAN_POINT('Ctrl Pts',(23.2939170635676,-2.36748782224901,-0.63054249811266));
#32298=CARTESIAN_POINT('Ctrl Pts',(23.3883527506744,-1.78622433682909,-2.0447933718034));
#32299=CARTESIAN_POINT('Ctrl Pts',(23.5347171694154,0.578777876478422,-2.72491209158622));
#32300=CARTESIAN_POINT('Ctrl Pts',(23.690503364318,2.58426961230329,-1.04031325744919));
#32301=CARTESIAN_POINT('Ctrl Pts',(23.8462895592206,2.30527110614996,1.56413143458517));
#32302=CARTESIAN_POINT('Ctrl Pts',(24.0020757541231,-0.0116548982896913,
2.78575885508703));
#32303=CARTESIAN_POINT('Ctrl Pts',(24.1371159370813,-2.01109387345396,1.71003568372357));
#32304=CARTESIAN_POINT('Ctrl Pts',(24.2202273884052,-2.36672388863589,0.464946474228187));
#32305=CARTESIAN_POINT('Ctrl Pts',(24.251410108095,-2.36878253894032,-0.00111285785031799));
#32306=CARTESIAN_POINT('Ctrl Pts',(23.448589891905,-2.36840991602323,-0.000688909241090621));
#32307=CARTESIAN_POINT('Ctrl Pts',(23.4714117840084,-2.36934544116764,-0.341925176311226));
#32308=CARTESIAN_POINT('Ctrl Pts',(23.546162407746,-2.1427579711721,-1.4584301293813));
#32309=CARTESIAN_POINT('Ctrl Pts',(23.6728417631177,-0.448717754286641,
-2.7494077907476));
#32310=CARTESIAN_POINT('Ctrl Pts',(23.8286279580203,2.03121191157331,-1.90653025915409));
#32311=CARTESIAN_POINT('Ctrl Pts',(23.9844141529229,2.7155240921129,0.621778103251025));
#32312=CARTESIAN_POINT('Ctrl Pts',(24.1402003478255,0.99925818313602,2.60041140430209));
#32313=CARTESIAN_POINT('Ctrl Pts',(24.2949255941528,-1.58266314056555,2.28242030819309));
#32314=CARTESIAN_POINT('Ctrl Pts',(24.397722108846,-2.37404568264673,0.754617836129284));
#32315=CARTESIAN_POINT('Ctrl Pts',(24.448589891905,-2.37530525058753,-0.000270455844553585));
#32316=CARTESIAN_POINT('Origin',(28.658,3.51939854619125E-16,0.));
#32317=CARTESIAN_POINT('',(28.658,0.261701021631923,2.93033728012268));
#32318=CARTESIAN_POINT('Ctrl Pts',(28.658,1.97801633036407,-1.31405326343373));
#32319=CARTESIAN_POINT('Ctrl Pts',(28.658,2.03588898944105,-1.24667939648802));
#32320=CARTESIAN_POINT('Ctrl Pts',(28.658,2.08963193546089,-1.17612088642746));
#32321=CARTESIAN_POINT('Ctrl Pts',(28.658,2.13887158382065,-1.10263113258862));
#32322=CARTESIAN_POINT('Ctrl Pts',(28.658,2.18456211831364,-1.03443840082659));
#32323=CARTESIAN_POINT('Ctrl Pts',(28.658,2.22637624274382,-0.963721068181632));
#32324=CARTESIAN_POINT('Ctrl Pts',(28.658,2.26436271250385,-0.890837075703206));
#32325=CARTESIAN_POINT('Ctrl Pts',(28.658,2.28264974318524,-0.855750061430627));
#32326=CARTESIAN_POINT('Ctrl Pts',(28.658,2.30004915173243,-0.82016034017639));
#32327=CARTESIAN_POINT('Ctrl Pts',(28.658,2.31656323187619,-0.784105041467371));
#32328=CARTESIAN_POINT('Ctrl Pts',(28.658,2.32355794425549,-0.768833440383695));
#32329=CARTESIAN_POINT('Ctrl Pts',(28.658,2.33039049782105,-0.75348540938221));
#32330=CARTESIAN_POINT('Ctrl Pts',(28.658,2.33705928183326,-0.738069100523836));
#32331=CARTESIAN_POINT('Ctrl Pts',(28.658,2.37145800155582,-0.658549163065291));
#32332=CARTESIAN_POINT('Ctrl Pts',(28.658,2.40152187518264,-0.577174196683355));
#32333=CARTESIAN_POINT('Ctrl Pts',(28.658,2.42731660870621,-0.494358545755739));
#32334=CARTESIAN_POINT('Ctrl Pts',(28.658,2.44988700053934,-0.421894851194075));
#32335=CARTESIAN_POINT('Ctrl Pts',(28.658,2.4691883185794,-0.348327044796147));
#32336=CARTESIAN_POINT('Ctrl Pts',(28.658,2.48523726885309,-0.273910862226402));
#32337=CARTESIAN_POINT('Ctrl Pts',(28.658,2.49043040451315,-0.249831198148779));
#32338=CARTESIAN_POINT('Ctrl Pts',(28.658,2.49528279533436,-0.225662577407877));
#32339=CARTESIAN_POINT('Ctrl Pts',(28.658,2.49979440405724,-0.20141333897661));
#32340=CARTESIAN_POINT('Ctrl Pts',(28.658,2.50272209611502,-0.185677421452916));
#32341=CARTESIAN_POINT('Ctrl Pts',(28.658,2.505506277858,-0.169907552756416));
#32342=CARTESIAN_POINT('Ctrl Pts',(28.658,2.50814687055771,-0.154105984441464));
#32343=CARTESIAN_POINT('Ctrl Pts',(28.658,2.51064326407261,-0.139167318333947));
#32344=CARTESIAN_POINT('Ctrl Pts',(28.658,2.51300962758955,-0.124210424344307));
#32345=CARTESIAN_POINT('Ctrl Pts',(28.658,2.51524622665656,-0.109238388801175));
#32346=CARTESIAN_POINT('Ctrl Pts',(28.658,2.52832241473202,-0.0217049745552181));
#32347=CARTESIAN_POINT('Ctrl Pts',(28.658,2.53696838029571,0.0663543248777591));
#32348=CARTESIAN_POINT('Ctrl Pts',(28.658,2.54124508921826,0.154537449743878));
#32349=CARTESIAN_POINT('Ctrl Pts',(28.658,2.54559508066862,0.244231615556881));
#32350=CARTESIAN_POINT('Ctrl Pts',(28.658,2.54542512050437,0.334054780156729));
#32351=CARTESIAN_POINT('Ctrl Pts',(28.658,2.54075262893098,0.423610145989604));
#32352=CARTESIAN_POINT('Ctrl Pts',(28.658,2.53686690572889,0.498085906388921));
#32353=CARTESIAN_POINT('Ctrl Pts',(28.658,2.52986651205561,0.572377218538135));
#32354=CARTESIAN_POINT('Ctrl Pts',(28.658,2.51973513979424,0.646262353103663));
#32355=CARTESIAN_POINT('Ctrl Pts',(28.658,2.51206070500465,0.702229761319919));
#32356=CARTESIAN_POINT('Ctrl Pts',(28.658,2.50258925346803,0.757964265454546));
#32357=CARTESIAN_POINT('Ctrl Pts',(28.658,2.4913040926272,0.813369424344011));
#32358=CARTESIAN_POINT('Ctrl Pts',(28.658,2.48766360830947,0.831242595573295));
#32359=CARTESIAN_POINT('Ctrl Pts',(28.658,2.483833274489,0.849085598142948));
#32360=CARTESIAN_POINT('Ctrl Pts',(28.658,2.4798188815792,0.866867679946036));
#32361=CARTESIAN_POINT('Ctrl Pts',(28.658,2.45941681290693,0.957240312180452));
#32362=CARTESIAN_POINT('Ctrl Pts',(28.658,2.43424071557649,1.04616757295001));
#32363=CARTESIAN_POINT('Ctrl Pts',(28.658,2.40432126657836,1.13323420516507));
#32364=CARTESIAN_POINT('Ctrl Pts',(28.658,2.38610167626726,1.18625384362247));
#32365=CARTESIAN_POINT('Ctrl Pts',(28.658,2.3661221590081,1.23858386635697));
#32366=CARTESIAN_POINT('Ctrl Pts',(28.658,2.34438027030047,1.29013186517359));
#32367=CARTESIAN_POINT('Ctrl Pts',(28.658,2.30980500483014,1.37210660837625));
#32368=CARTESIAN_POINT('Ctrl Pts',(28.658,2.27077563476682,1.45210464318559));
#32369=CARTESIAN_POINT('Ctrl Pts',(28.658,2.22760963761098,1.52996848770481));
#32370=CARTESIAN_POINT('Ctrl Pts',(28.658,2.20262999297066,1.57502736030302));
#32371=CARTESIAN_POINT('Ctrl Pts',(28.658,2.17626409255244,1.61937133560154));
#32372=CARTESIAN_POINT('Ctrl Pts',(28.658,2.14856603599913,1.66296748678073));
#32373=CARTESIAN_POINT('Ctrl Pts',(28.658,2.1288093227664,1.69406413268585));
#32374=CARTESIAN_POINT('Ctrl Pts',(28.658,2.10837472156678,1.72478026212631));
#32375=CARTESIAN_POINT('Ctrl Pts',(28.658,2.0872803454754,1.75510318279917));
#32376=CARTESIAN_POINT('Ctrl Pts',(28.658,2.07669314170718,1.77032216527205));
#32377=CARTESIAN_POINT('Ctrl Pts',(28.658,2.06593715859879,1.78544543077647));
#32378=CARTESIAN_POINT('Ctrl Pts',(28.658,2.05503140742641,1.80044869555866));
#32379=CARTESIAN_POINT('Ctrl Pts',(28.658,2.00068115281266,1.87521945165428));
#32380=CARTESIAN_POINT('Ctrl Pts',(28.658,1.94254510232413,1.9471157067966));
#32381=CARTESIAN_POINT('Ctrl Pts',(28.658,1.88099648476523,2.01598109009273));
#32382=CARTESIAN_POINT('Ctrl Pts',(28.658,1.81824029970113,2.08619759389164));
#32383=CARTESIAN_POINT('Ctrl Pts',(28.658,1.75193589590128,2.15326379417956));
#32384=CARTESIAN_POINT('Ctrl Pts',(28.658,1.68242589079217,2.21699709023191));
#32385=CARTESIAN_POINT('Ctrl Pts',(28.658,1.61227576386633,2.28131731003994));
#32386=CARTESIAN_POINT('Ctrl Pts',(28.658,1.53886014435481,2.34224366390707));
#32387=CARTESIAN_POINT('Ctrl Pts',(28.658,1.46248554098919,2.39956107936614));
#32388=CARTESIAN_POINT('Ctrl Pts',(28.658,1.41833873564515,2.43269226004124));
#32389=CARTESIAN_POINT('Ctrl Pts',(28.658,1.37320247880795,2.46461706605157));
#32390=CARTESIAN_POINT('Ctrl Pts',(28.658,1.32713029596024,2.49528840587952));
#32391=CARTESIAN_POINT('Ctrl Pts',(28.658,1.31488967467329,2.5034372764559));
#32392=CARTESIAN_POINT('Ctrl Pts',(28.658,1.30258075027275,2.511499067118));
#32393=CARTESIAN_POINT('Ctrl Pts',(28.658,1.29021178873854,2.51946814645669));
#32394=CARTESIAN_POINT('Ctrl Pts',(28.658,1.20764107863156,2.57266683561706));
#32395=CARTESIAN_POINT('Ctrl Pts',(28.658,1.12259640491928,2.62161093215467));
#32396=CARTESIAN_POINT('Ctrl Pts',(28.658,1.03544610319146,2.66611476104981));
#32397=CARTESIAN_POINT('Ctrl Pts',(28.658,0.947976267227596,2.71078176203599));
#32398=CARTESIAN_POINT('Ctrl Pts',(28.658,0.858384645681997,2.75097657191429));
#32399=CARTESIAN_POINT('Ctrl Pts',(28.658,0.76700170558157,2.7864795973746));
#32400=CARTESIAN_POINT('Ctrl Pts',(28.658,0.677259469945933,2.82134519562669));
#32401=CARTESIAN_POINT('Ctrl Pts',(28.658,0.585788889330719,2.85168650745828));
#32402=CARTESIAN_POINT('Ctrl Pts',(28.658,0.492873620233273,2.87725594522238));
#32403=CARTESIAN_POINT('Ctrl Pts',(28.658,0.416738026937611,2.89820776867741));
#32404=CARTESIAN_POINT('Ctrl Pts',(28.658,0.339631723233453,2.91595505282006));
#32405=CARTESIAN_POINT('Ctrl Pts',(28.658,0.261701021631923,2.93033728012268));
#32406=CARTESIAN_POINT('',(28.658,-2.942,-3.60291088309151E-16));
#32407=CARTESIAN_POINT('Origin',(28.658,0.,0.));
#32408=CARTESIAN_POINT('',(28.658,-2.15060832247059,2.01293848078683));
#32409=CARTESIAN_POINT('Origin',(28.658,0.,0.));
#32410=CARTESIAN_POINT('Ctrl Pts',(28.658,-2.15060832247059,2.01293848078683));
#32411=CARTESIAN_POINT('Ctrl Pts',(28.658,-2.20971109593349,1.93767297749437));
#32412=CARTESIAN_POINT('Ctrl Pts',(28.658,-2.26481658708665,1.85956683039048));
#32413=CARTESIAN_POINT('Ctrl Pts',(28.658,-2.31558252285751,1.77874869425101));
#32414=CARTESIAN_POINT('Ctrl Pts',(28.658,-2.32237888851895,1.76792904526908));
#32415=CARTESIAN_POINT('Ctrl Pts',(28.658,-2.32909740761893,1.75706075632002));
#32416=CARTESIAN_POINT('Ctrl Pts',(28.658,-2.33573719302841,1.74614410673189));
#32417=CARTESIAN_POINT('Ctrl Pts',(28.658,-2.38668022372525,1.66238730123612));
#32418=CARTESIAN_POINT('Ctrl Pts',(28.658,-2.43299277513564,1.57578453084994));
#32419=CARTESIAN_POINT('Ctrl Pts',(28.658,-2.47464052311135,1.48675406675739));
#32420=CARTESIAN_POINT('Ctrl Pts',(28.658,-2.48689377831249,1.46056026156441));
#32421=CARTESIAN_POINT('Ctrl Pts',(28.658,-2.49874290551813,1.43415626299096));
#32422=CARTESIAN_POINT('Ctrl Pts',(28.658,-2.51018618118443,1.40755265714468));
#32423=CARTESIAN_POINT('Ctrl Pts',(28.658,-2.51771390631931,1.39005201849476));
#32424=CARTESIAN_POINT('Ctrl Pts',(28.658,-2.52506599547472,1.37246500180567));
#32425=CARTESIAN_POINT('Ctrl Pts',(28.658,-2.53224186714647,1.35479462666926));
#32426=CARTESIAN_POINT('Ctrl Pts',(28.658,-2.53962113906836,1.33662338433687));
#32427=CARTESIAN_POINT('Ctrl Pts',(28.658,-2.54681097419375,1.31837145371668));
#32428=CARTESIAN_POINT('Ctrl Pts',(28.658,-2.55380852110088,1.30004960134548));
#32429=CARTESIAN_POINT('Ctrl Pts',(28.658,-2.58844585274772,1.20935780815165));
#32430=CARTESIAN_POINT('Ctrl Pts',(28.658,-2.61839882158235,1.11689744862561));
#32431=CARTESIAN_POINT('Ctrl Pts',(28.658,-2.64365122411707,1.02308128352135));
#32432=CARTESIAN_POINT('Ctrl Pts',(28.658,-2.66475485704852,0.944678370821319));
#32433=CARTESIAN_POINT('Ctrl Pts',(28.658,-2.68257463739759,0.865327992912511));
#32434=CARTESIAN_POINT('Ctrl Pts',(28.658,-2.69707318068004,0.785271122320479));
#32435=CARTESIAN_POINT('Ctrl Pts',(28.658,-2.70352672731022,0.749636456315314));
#32436=CARTESIAN_POINT('Ctrl Pts',(28.658,-2.70932190569519,0.713861857690371));
#32437=CARTESIAN_POINT('Ctrl Pts',(28.658,-2.7144538141254,0.677968940347287));
#32438=CARTESIAN_POINT('Ctrl Pts',(28.658,-2.71700175179471,0.660148490624957));
#32439=CARTESIAN_POINT('Ctrl Pts',(28.658,-2.71938617708855,0.642298879916618));
#32440=CARTESIAN_POINT('Ctrl Pts',(28.658,-2.72160640006766,0.624422786102583));
#32441=CARTESIAN_POINT('Ctrl Pts',(28.658,-2.72363648596765,0.608077578283332));
#32442=CARTESIAN_POINT('Ctrl Pts',(28.658,-2.72552824448812,0.591718366592941));
#32443=CARTESIAN_POINT('Ctrl Pts',(28.658,-2.72728098621858,0.575353162719347));
#32444=CARTESIAN_POINT('Ctrl Pts',(28.658,-2.73739781604062,0.480893163442538));
#32445=CARTESIAN_POINT('Ctrl Pts',(28.658,-2.74289532062776,0.386169908251331));
#32446=CARTESIAN_POINT('Ctrl Pts',(28.658,-2.7437548509834,0.291566670300918));
#32447=CARTESIAN_POINT('Ctrl Pts',(28.658,-2.74460687110618,0.197790037650447));
#32448=CARTESIAN_POINT('Ctrl Pts',(28.658,-2.74090146504082,0.104130391083328));
#32449=CARTESIAN_POINT('Ctrl Pts',(28.658,-2.73257054458709,0.010970921487669));
#32450=CARTESIAN_POINT('Ctrl Pts',(28.658,-2.72570835794339,-0.065764617105541));
#32451=CARTESIAN_POINT('Ctrl Pts',(28.658,-2.7157069180874,-0.142160847495387));
#32452=CARTESIAN_POINT('Ctrl Pts',(28.658,-2.70250334697467,-0.217991837109981));
#32453=CARTESIAN_POINT('Ctrl Pts',(28.658,-2.69260066864013,-0.274865079320927));
#32454=CARTESIAN_POINT('Ctrl Pts',(28.658,-2.68089633000001,-0.331420179713332));
#32455=CARTESIAN_POINT('Ctrl Pts',(28.658,-2.66735565981843,-0.387555995282867));
#32456=CARTESIAN_POINT('Ctrl Pts',(28.658,-2.66394701524533,-0.401687278338419));
#32457=CARTESIAN_POINT('Ctrl Pts',(28.658,-2.66042196824992,-0.415791962607326));
#32458=CARTESIAN_POINT('Ctrl Pts',(28.658,-2.65677989678547,-0.429868374047563));
#32459=CARTESIAN_POINT('Ctrl Pts',(28.658,-2.65341425236481,-0.442876409746268));
#32460=CARTESIAN_POINT('Ctrl Pts',(28.658,-2.64994974372578,-0.455856001451419));
#32461=CARTESIAN_POINT('Ctrl Pts',(28.658,-2.64638824974718,-0.468798346640149));
#32462=CARTESIAN_POINT('Ctrl Pts',(28.658,-2.62270732724449,-0.554853994988378));
#32463=CARTESIAN_POINT('Ctrl Pts',(28.658,-2.59471590580757,-0.639367325882882));
#32464=CARTESIAN_POINT('Ctrl Pts',(28.658,-2.56235842010114,-0.7219999177347));
#32465=CARTESIAN_POINT('Ctrl Pts',(28.658,-2.54209052173618,-0.773758851926326));
#32466=CARTESIAN_POINT('Ctrl Pts',(28.658,-2.52010870092681,-0.824779529231049));
#32467=CARTESIAN_POINT('Ctrl Pts',(28.658,-2.4963902536118,-0.874973476494181));
#32468=CARTESIAN_POINT('Ctrl Pts',(28.658,-2.45769064340973,-0.956871172738262));
#32469=CARTESIAN_POINT('Ctrl Pts',(28.658,-2.41436920801051,-1.03657008506992));
#32470=CARTESIAN_POINT('Ctrl Pts',(28.658,-2.36672566050128,-1.11382437417113));
#32471=CARTESIAN_POINT('Ctrl Pts',(28.658,-2.31891811374559,-1.19134458900331));
#32472=CARTESIAN_POINT('Ctrl Pts',(28.658,-2.2667577640464,-1.26640389984806));
#32473=CARTESIAN_POINT('Ctrl Pts',(28.658,-2.21051982316866,-1.33870955140761));
#32474=CARTESIAN_POINT('Ctrl Pts',(28.658,-2.20189537756213,-1.34979808255201));
#32475=CARTESIAN_POINT('Ctrl Pts',(28.658,-2.19318006476582,-1.36081520380594));
#32476=CARTESIAN_POINT('Ctrl Pts',(28.658,-2.18437794934293,-1.37175665419369));
#32477=CARTESIAN_POINT('Ctrl Pts',(28.658,-2.12879717302225,-1.4408462170326));
#32478=CARTESIAN_POINT('Ctrl Pts',(28.658,-2.06972321612038,-1.50696694812369));
#32479=CARTESIAN_POINT('Ctrl Pts',(28.658,-2.0074651266359,-1.5699147697608));
#32480=CARTESIAN_POINT('Ctrl Pts',(28.658,-1.9452667315866,-1.63280223563227));
#32481=CARTESIAN_POINT('Ctrl Pts',(28.658,-1.87988940823054,-1.69252336443322));
#32482=CARTESIAN_POINT('Ctrl Pts',(28.658,-1.81161260297583,-1.74883157744085));
#32483=CARTESIAN_POINT('Ctrl Pts',(28.658,-1.74439799581986,-1.8042637905159));
#32484=CARTESIAN_POINT('Ctrl Pts',(28.658,-1.67437256396589,-1.85638878596463));
#32485=CARTESIAN_POINT('Ctrl Pts',(28.658,-1.60178815117267,-1.9049236123197));
#32486=CARTESIAN_POINT('Ctrl Pts',(28.658,-1.57702435474135,-1.92148235425112));
#32487=CARTESIAN_POINT('Ctrl Pts',(28.658,-1.55196262566561,-1.93762276924518));
#32488=CARTESIAN_POINT('Ctrl Pts',(28.658,-1.52661283080042,-1.95333221692257));
#32489=CARTESIAN_POINT('Ctrl Pts',(28.658,-1.5105418481757,-1.96329151884236));
#32490=CARTESIAN_POINT('Ctrl Pts',(28.658,-1.49435508656289,-1.97307759307412));
#32491=CARTESIAN_POINT('Ctrl Pts',(28.658,-1.47805506249159,-1.98268706081389));
#32492=CARTESIAN_POINT('Ctrl Pts',(28.658,-1.46641505727283,-1.98954927489106));
#32493=CARTESIAN_POINT('Ctrl Pts',(28.658,-1.45472491992427,-1.99631691153973));
#32494=CARTESIAN_POINT('Ctrl Pts',(28.658,-1.44298829166971,-2.00298769190301));
#32495=CARTESIAN_POINT('Ctrl Pts',(28.658,-1.3688399031693,-2.04513161972017));
#32496=CARTESIAN_POINT('Ctrl Pts',(28.658,-1.2928037819447,-2.08343336979007));
#32497=CARTESIAN_POINT('Ctrl Pts',(28.658,-1.21513616067108,-2.11767523333238));
#32498=CARTESIAN_POINT('Ctrl Pts',(28.658,-1.13866984115548,-2.15138747062637));
#32499=CARTESIAN_POINT('Ctrl Pts',(28.658,-1.06062131430581,-2.18116469203935));
#32500=CARTESIAN_POINT('Ctrl Pts',(28.658,-0.981226066391064,-2.20675022144869));
#32501=CARTESIAN_POINT('Ctrl Pts',(28.658,-0.904293774038269,-2.23154205068555));
#32502=CARTESIAN_POINT('Ctrl Pts',(28.658,-0.826096380893346,-2.25239828191146));
#32503=CARTESIAN_POINT('Ctrl Pts',(28.658,-0.74684990431363,-2.26903704779655));
#32504=CARTESIAN_POINT('Ctrl Pts',(28.658,-0.69773198312443,-2.27934995540711));
#32505=CARTESIAN_POINT('Ctrl Pts',(28.658,-0.648211111266871,-2.28804169467426));
#32506=CARTESIAN_POINT('Ctrl Pts',(28.658,-0.598340649004787,-2.29503519150547));
#32507=CARTESIAN_POINT('Ctrl Pts',(22.2707660089946,-1.03908919352505,2.13201587949046));
#32508=CARTESIAN_POINT('Ctrl Pts',(22.3226947406288,-1.73471873725821,1.79298409809367));
#32509=CARTESIAN_POINT('Ctrl Pts',(22.4265522038972,-2.75780127841751,0.387620901480232));
#32510=CARTESIAN_POINT('Ctrl Pts',(22.5823383987998,-1.85932621210726,-2.07658872801938));
#32511=CARTESIAN_POINT('Ctrl Pts',(22.7381245937023,0.68524861492584,-2.6995454694093));
#32512=CARTESIAN_POINT('Ctrl Pts',(22.8939107886049,2.62282735660906,-0.938746401795666));
#32513=CARTESIAN_POINT('Ctrl Pts',(23.0496969835074,2.24240074214882,1.65328021767869));
#32514=CARTESIAN_POINT('Ctrl Pts',(23.2054831784101,-0.120664916242889,
2.78308709983206));
#32515=CARTESIAN_POINT('Ctrl Pts',(23.3612693733126,-2.37689989423139,1.45294520051045));
#32516=CARTESIAN_POINT('Ctrl Pts',(23.5170555682152,-2.53199390158006,-1.16180500434049));
#32517=CARTESIAN_POINT('Ctrl Pts',(23.6728417631177,-0.448717754286641,
-2.7494077907476));
#32518=CARTESIAN_POINT('Ctrl Pts',(23.8286279580203,2.03121191157331,-1.90653025915409));
#32519=CARTESIAN_POINT('Ctrl Pts',(23.9844141529229,2.7155240921129,0.621778103251025));
#32520=CARTESIAN_POINT('Ctrl Pts',(24.1402003478255,0.99925818313602,2.60041140430209));
#32521=CARTESIAN_POINT('Ctrl Pts',(24.295986542728,-1.60036733438438,2.28023984825943));
#32522=CARTESIAN_POINT('Ctrl Pts',(24.4517727376306,-2.78524046876828,-0.0557082387313367));
#32523=CARTESIAN_POINT('Ctrl Pts',(24.6075589325332,-1.50790971480175,-2.34240766296688));
#32524=CARTESIAN_POINT('Ctrl Pts',(24.7633451274357,1.10244025446093,-2.55837695905924));
#32525=CARTESIAN_POINT('Ctrl Pts',(24.9191313223383,2.738213197235,-0.512694142435889));
#32526=CARTESIAN_POINT('Ctrl Pts',(25.0749175172409,1.95335583875086,1.98621940187114));
#32527=CARTESIAN_POINT('Ctrl Pts',(25.2307037121435,-0.558303519624818,
2.72927902174966));
#32528=CARTESIAN_POINT('Ctrl Pts',(25.386489907046,-2.5764124445433,1.0596063475242));
#32529=CARTESIAN_POINT('Ctrl Pts',(25.5422761019486,-2.31692596255169,-1.54677754708461));
#32530=CARTESIAN_POINT('Ctrl Pts',(25.6980622968511,-0.00923482980258066,
-2.78578202961156));
#32531=CARTESIAN_POINT('Ctrl Pts',(25.8538484917537,2.30662002902024,-1.5621045377548));
#32532=CARTESIAN_POINT('Ctrl Pts',(26.0096346866563,2.58338094683827,1.04250164542461));
#32533=CARTESIAN_POINT('Ctrl Pts',(26.1654208815589,0.576386046271133,2.72551762147395));
#32534=CARTESIAN_POINT('Ctrl Pts',(26.3212070764614,-1.94014432814736,1.99912614746469));
#32535=CARTESIAN_POINT('Ctrl Pts',(26.476993271364,-2.7415523872825,-0.494528446616266));
#32536=CARTESIAN_POINT('Ctrl Pts',(26.6327794662666,-1.11937732072311,-2.55101230581224));
#32537=CARTESIAN_POINT('Ctrl Pts',(26.7885656611692,1.49234563926014,-2.35235220176952));
#32538=CARTESIAN_POINT('Ctrl Pts',(26.9443518560717,2.78481186300027,-0.0741754152063169));
#32539=CARTESIAN_POINT('Ctrl Pts',(27.1001380509743,1.61544610555625,2.26958439782059));
#32540=CARTESIAN_POINT('Ctrl Pts',(27.2559242458769,-0.981988199781967,
2.60696950467868));
#32541=CARTESIAN_POINT('Ctrl Pts',(27.4117104407795,-2.71135690270178,0.639787255203349));
#32542=CARTESIAN_POINT('Ctrl Pts',(27.567496635682,-2.04377823479325,-1.89305926739468));
#32543=CARTESIAN_POINT('Ctrl Pts',(27.7232828305846,0.430422244683163,-2.75224826615359));
#32544=CARTESIAN_POINT('Ctrl Pts',(27.8790690254871,2.52434834774427,-1.17871200290743));
#32545=CARTESIAN_POINT('Ctrl Pts',(28.0348552203897,2.38625876548845,1.43744121743837));
#32546=CARTESIAN_POINT('Ctrl Pts',(28.1906414152923,0.139550436043699,2.78166084946855));
#32547=CARTESIAN_POINT('Ctrl Pts',(28.3464276101949,-2.2322534987586,1.66923905587135));
#32548=CARTESIAN_POINT('Ctrl Pts',(28.5022138050974,-2.62724420518177,-0.923745495709923));
#32549=CARTESIAN_POINT('Ctrl Pts',(28.6060712683658,-1.34715978233134,-2.09980989479535));
#32550=CARTESIAN_POINT('Ctrl Pts',(28.658,-0.598340649004787,-2.29503519150547));
#32551=CARTESIAN_POINT('Ctrl Pts',(22.3805106726631,-1.12236674703443,2.3028857793927));
#32552=CARTESIAN_POINT('Ctrl Pts',(22.4324394042973,-1.87374735324802,1.93668237741455));
#32553=CARTESIAN_POINT('Ctrl Pts',(22.5362968675657,-2.97882459861252,0.418686685404777));
#32554=CARTESIAN_POINT('Ctrl Pts',(22.6920830624682,-2.00834146420018,-2.24301643219745));
#32555=CARTESIAN_POINT('Ctrl Pts',(22.8478692573708,0.740167700363659,-2.91589989180214));
#32556=CARTESIAN_POINT('Ctrl Pts',(23.0036554522733,2.83303322430258,-1.0139820063948));
#32557=CARTESIAN_POINT('Ctrl Pts',(23.1594416471759,2.42211741032076,1.78578196310313));
#32558=CARTESIAN_POINT('Ctrl Pts',(23.3152278420785,-0.130335576934711,
3.00613694610299));
#32559=CARTESIAN_POINT('Ctrl Pts',(23.4710140369811,-2.56739596459932,1.56939114416543));
#32560=CARTESIAN_POINT('Ctrl Pts',(23.6268002318836,-2.73491994386615,-1.25491758699396));
#32561=CARTESIAN_POINT('Ctrl Pts',(23.7825864267862,-0.484680130785283,
-2.96975841689198));
#32562=CARTESIAN_POINT('Ctrl Pts',(23.9383726216888,2.19400290171065,-2.0593286682448));
#32563=CARTESIAN_POINT('Ctrl Pts',(24.0941588165914,2.93315911737939,0.671610359795614));
#32564=CARTESIAN_POINT('Ctrl Pts',(24.2499450114939,1.07934348989732,2.80882075088911));
#32565=CARTESIAN_POINT('Ctrl Pts',(24.4057312063965,-1.72862838950299,2.46298912249013));
#32566=CARTESIAN_POINT('Ctrl Pts',(24.561517401299,-3.00846289627471,-0.0601729621263726));
#32567=CARTESIAN_POINT('Ctrl Pts',(24.7173035962016,-1.62876077623539,-2.53013936175565));
#32568=CARTESIAN_POINT('Ctrl Pts',(24.8730897911042,1.1907950635128,-2.76341746514174));
#32569=CARTESIAN_POINT('Ctrl Pts',(25.0288759860068,2.95766663537466,-0.553783891176143));
#32570=CARTESIAN_POINT('Ctrl Pts',(25.1846621809093,2.10990707265658,2.1454044781393));
#32571=CARTESIAN_POINT('Ctrl Pts',(25.3404483758119,-0.603048620930609,
2.94801643254376));
#32572=CARTESIAN_POINT('Ctrl Pts',(25.4962345707145,-2.78289840027231,1.14452824340639));
#32573=CARTESIAN_POINT('Ctrl Pts',(25.652020765617,-2.50261543658917,-1.67074366158866));
#32574=CARTESIAN_POINT('Ctrl Pts',(25.8078069605196,-0.00997495301609062,
-3.00904786038153));
#32575=CARTESIAN_POINT('Ctrl Pts',(25.9635931554222,2.49148353649345,-1.68729903023991));
#32576=CARTESIAN_POINT('Ctrl Pts',(26.1193793503248,2.79042539150775,1.12605268907077));
#32577=CARTESIAN_POINT('Ctrl Pts',(26.2751655452273,0.622580367326068,2.94395357574758));
#32578=CARTESIAN_POINT('Ctrl Pts',(26.4309517401299,-2.09563672871319,2.15934563175432));
#32579=CARTESIAN_POINT('Ctrl Pts',(26.5867379350324,-2.96127344400544,-0.534162310033983));
#32580=CARTESIAN_POINT('Ctrl Pts',(26.7425241299351,-1.20908954687713,-2.7554625735315));
#32581=CARTESIAN_POINT('Ctrl Pts',(26.8983103248376,1.61194932160273,-2.54088090322894));
#32582=CARTESIAN_POINT('Ctrl Pts',(27.0540965197402,3.0079999400005,-0.0801201860185042));
#32583=CARTESIAN_POINT('Ctrl Pts',(27.2098827146428,1.74491564516392,2.45147969353855));
#32584=CARTESIAN_POINT('Ctrl Pts',(27.3656689095453,-1.06068940788086,2.81590444864312));
#32585=CARTESIAN_POINT('Ctrl Pts',(27.5214551044479,-2.92865794957514,0.691062850899878));
#32586=CARTESIAN_POINT('Ctrl Pts',(27.6772412993505,-2.20757634988279,-2.04477804709066));
#32587=CARTESIAN_POINT('Ctrl Pts',(27.833027494253,0.464918331964785,-2.97282654151624));
#32588=CARTESIAN_POINT('Ctrl Pts',(27.9888136891556,2.72666163895697,-1.27317959289484));
#32589=CARTESIAN_POINT('Ctrl Pts',(28.1445998840582,2.57750490034244,1.55264459809882));
#32590=CARTESIAN_POINT('Ctrl Pts',(28.3003860789608,0.150734672177907,3.00459638924711));
#32591=CARTESIAN_POINT('Ctrl Pts',(28.4561722738633,-2.41115691854948,1.80301981854457));
#32592=CARTESIAN_POINT('Ctrl Pts',(28.6119584687659,-2.83780406014188,-0.997778856298598));
#32593=CARTESIAN_POINT('Ctrl Pts',(28.7158159320343,-1.45512757908823,-2.26809865379989));
#32594=CARTESIAN_POINT('Ctrl Pts',(28.7677446636685,-0.646294516415629,
-2.47897023496227));
#32595=CARTESIAN_POINT('Ctrl Pts',(22.4902553363315,-1.20564430054382,2.47375567929494));
#32596=CARTESIAN_POINT('Ctrl Pts',(22.5421840679657,-2.01277596923782,2.08038065673544));
#32597=CARTESIAN_POINT('Ctrl Pts',(22.6460415312341,-3.19984791880754,0.449752469329321));
#32598=CARTESIAN_POINT('Ctrl Pts',(22.8018277261367,-2.1573567162931,-2.40944413637552));
#32599=CARTESIAN_POINT('Ctrl Pts',(22.9576139210393,0.795086785801479,-3.13225431419499));
#32600=CARTESIAN_POINT('Ctrl Pts',(23.1134001159418,3.0432390919961,-1.08921761099393));
#32601=CARTESIAN_POINT('Ctrl Pts',(23.2691863108444,2.6018340784927,1.91828370852757));
#32602=CARTESIAN_POINT('Ctrl Pts',(23.4249725057469,-0.140006237626535,
3.22918679237392));
#32603=CARTESIAN_POINT('Ctrl Pts',(23.5807587006495,-2.75789203496725,1.68583708782041));
#32604=CARTESIAN_POINT('Ctrl Pts',(23.7365448955521,-2.93784598615223,-1.34803016964744));
#32605=CARTESIAN_POINT('Ctrl Pts',(23.8923310904547,-0.520642507283926,
-3.19010904303636));
#32606=CARTESIAN_POINT('Ctrl Pts',(24.0481172853572,2.35679389184798,-2.2121270773355));
#32607=CARTESIAN_POINT('Ctrl Pts',(24.2039034802598,3.15079414264587,0.721442616340202));
#32608=CARTESIAN_POINT('Ctrl Pts',(24.3596896751624,1.15942879665862,3.01723009747613));
#32609=CARTESIAN_POINT('Ctrl Pts',(24.515475870065,-1.8568894446216,2.64573839672082));
#32610=CARTESIAN_POINT('Ctrl Pts',(24.6712620649675,-3.23168532378114,-0.0646376855214102));
#32611=CARTESIAN_POINT('Ctrl Pts',(24.8270482598701,-1.74961183766903,-2.71787106054443));
#32612=CARTESIAN_POINT('Ctrl Pts',(24.9828344547727,1.27914987256467,-2.96845797122425));
#32613=CARTESIAN_POINT('Ctrl Pts',(25.1386206496752,3.17712007351433,-0.594873639916395));
#32614=CARTESIAN_POINT('Ctrl Pts',(25.2944068445778,2.26645830656231,2.30458955440746));
#32615=CARTESIAN_POINT('Ctrl Pts',(25.4501930394804,-0.647793722236402,
3.16675384333786));
#32616=CARTESIAN_POINT('Ctrl Pts',(25.6059792343829,-2.98938435600131,1.22945013928857));
#32617=CARTESIAN_POINT('Ctrl Pts',(25.7617654292856,-2.68830491062663,-1.79470977609272));
#32618=CARTESIAN_POINT('Ctrl Pts',(25.9175516241881,-0.0107150762296046,
-3.23231369115149));
#32619=CARTESIAN_POINT('Ctrl Pts',(26.0733378190907,2.67634704396667,-1.81249352272502));
#32620=CARTESIAN_POINT('Ctrl Pts',(26.2291240139932,2.99746983617723,1.20960373271694));
#32621=CARTESIAN_POINT('Ctrl Pts',(26.3849102088958,0.668774688381005,3.16238953002122));
#32622=CARTESIAN_POINT('Ctrl Pts',(26.5406964037984,-2.25112912927902,2.31956511604394));
#32623=CARTESIAN_POINT('Ctrl Pts',(26.6964825987009,-3.18099450072837,-0.573796173451701));
#32624=CARTESIAN_POINT('Ctrl Pts',(26.8522687936035,-1.29880177303115,-2.95991284125075));
#32625=CARTESIAN_POINT('Ctrl Pts',(27.0080549885061,1.73155300394531,-2.72940960468835));
#32626=CARTESIAN_POINT('Ctrl Pts',(27.1638411834086,3.23118801700073,-0.0860649568306912));
#32627=CARTESIAN_POINT('Ctrl Pts',(27.3196273783112,1.87438518477158,2.6333749892565));
#32628=CARTESIAN_POINT('Ctrl Pts',(27.4754135732138,-1.13939061597976,3.02483939260757));
#32629=CARTESIAN_POINT('Ctrl Pts',(27.6311997681164,-3.14595899644851,0.742338446596407));
#32630=CARTESIAN_POINT('Ctrl Pts',(27.7869859630189,-2.37137446497233,-2.19649682678664));
#32631=CARTESIAN_POINT('Ctrl Pts',(27.9427721579215,0.499414419246406,-3.19340481687888));
#32632=CARTESIAN_POINT('Ctrl Pts',(28.098558352824,2.92897493016967,-1.36764718288226));
#32633=CARTESIAN_POINT('Ctrl Pts',(28.2543445477267,2.76875103519641,1.66784797875926));
#32634=CARTESIAN_POINT('Ctrl Pts',(28.4101307426292,0.161918908312118,3.22753192902568));
#32635=CARTESIAN_POINT('Ctrl Pts',(28.5659169375318,-2.59006033834036,1.93680058121779));
#32636=CARTESIAN_POINT('Ctrl Pts',(28.7217031324344,-3.04836391510199,-1.07181221688727));
#32637=CARTESIAN_POINT('Ctrl Pts',(28.8255605957027,-1.56309537584512,-2.43638741280443));
#32638=CARTESIAN_POINT('Ctrl Pts',(28.8774893273369,-0.69424838382647,-2.66290527841906));
#32639=CARTESIAN_POINT('Ctrl Pts',(22.6,-1.2889218540532,2.64462557919719));
#32640=CARTESIAN_POINT('Ctrl Pts',(22.6519287316342,-2.15180458522763,2.22407893605632));
#32641=CARTESIAN_POINT('Ctrl Pts',(22.7557861949026,-3.42087123900255,0.480818253253867));
#32642=CARTESIAN_POINT('Ctrl Pts',(22.9115723898051,-2.30637196838603,-2.5758718405536));
#32643=CARTESIAN_POINT('Ctrl Pts',(23.0673585847077,0.850005871239299,-3.34860873658782));
#32644=CARTESIAN_POINT('Ctrl Pts',(23.2231447796103,3.25344495968962,-1.16445321559307));
#32645=CARTESIAN_POINT('Ctrl Pts',(23.3789309745129,2.78155074666463,2.05078545395201));
#32646=CARTESIAN_POINT('Ctrl Pts',(23.5347171694154,-0.149676898318359,
3.45223663864485));
#32647=CARTESIAN_POINT('Ctrl Pts',(23.690503364318,-2.94838810533518,1.80228303147539));
#32648=CARTESIAN_POINT('Ctrl Pts',(23.8462895592206,-3.14077202843831,-1.44114275230091));
#32649=CARTESIAN_POINT('Ctrl Pts',(24.0020757541232,-0.556604883782569,
-3.41045966918074));
#32650=CARTESIAN_POINT('Ctrl Pts',(24.1578619490257,2.51958488198532,-2.36492548642621));
#32651=CARTESIAN_POINT('Ctrl Pts',(24.3136481439283,3.36842916791236,0.77127487288479));
#32652=CARTESIAN_POINT('Ctrl Pts',(24.4694343388308,1.23951410341992,3.22563944406314));
#32653=CARTESIAN_POINT('Ctrl Pts',(24.6252205337334,-1.98515049974021,2.82848767095152));
#32654=CARTESIAN_POINT('Ctrl Pts',(24.781006728636,-3.45490775128757,-0.0691024089164465));
#32655=CARTESIAN_POINT('Ctrl Pts',(24.9367929235386,-1.87046289910267,-2.90560275933321));
#32656=CARTESIAN_POINT('Ctrl Pts',(25.0925791184411,1.36750468161654,-3.17349847730675));
#32657=CARTESIAN_POINT('Ctrl Pts',(25.2483653133437,3.39657351165399,-0.635963388656646));
#32658=CARTESIAN_POINT('Ctrl Pts',(25.4041515082463,2.42300954046803,2.46377463067561));
#32659=CARTESIAN_POINT('Ctrl Pts',(25.5599377031488,-0.692538823542196,
3.38549125413197));
#32660=CARTESIAN_POINT('Ctrl Pts',(25.7157238980514,-3.19587031173032,1.31437203517075));
#32661=CARTESIAN_POINT('Ctrl Pts',(25.871510092954,-2.87399438466411,-1.91867589059677));
#32662=CARTESIAN_POINT('Ctrl Pts',(26.0272962878565,-0.0114551994431134,
-3.45557952192146));
#32663=CARTESIAN_POINT('Ctrl Pts',(26.1830824827591,2.86121055143987,-1.93768801521013));
#32664=CARTESIAN_POINT('Ctrl Pts',(26.3388686776617,3.20451428084672,1.2931547763631));
#32665=CARTESIAN_POINT('Ctrl Pts',(26.4946548725642,0.714969009435938,3.38082548429487));
#32666=CARTESIAN_POINT('Ctrl Pts',(26.6504410674668,-2.40662152984485,2.47978460033357));
#32667=CARTESIAN_POINT('Ctrl Pts',(26.8062272623694,-3.4007155574513,-0.613430036869417));
#32668=CARTESIAN_POINT('Ctrl Pts',(26.962013457272,-1.38851399918516,-3.16436310897001));
#32669=CARTESIAN_POINT('Ctrl Pts',(27.1177996521745,1.8511566862879,-2.91793830614776));
#32670=CARTESIAN_POINT('Ctrl Pts',(27.2735858470772,3.45437609400096,-0.0920097276428782));
#32671=CARTESIAN_POINT('Ctrl Pts',(27.4293720419797,2.00385472437925,2.81527028497446));
#32672=CARTESIAN_POINT('Ctrl Pts',(27.5851582368823,-1.21809182407865,3.23377433657202));
#32673=CARTESIAN_POINT('Ctrl Pts',(27.7409444317848,-3.36326004332187,0.793614042292933));
#32674=CARTESIAN_POINT('Ctrl Pts',(27.8967306266874,-2.53517258006187,-2.34821560648262));
#32675=CARTESIAN_POINT('Ctrl Pts',(28.05251682159,0.533910506528028,-3.41398309224154));
#32676=CARTESIAN_POINT('Ctrl Pts',(28.2083030164925,3.13128822138237,-1.46211477286968));
#32677=CARTESIAN_POINT('Ctrl Pts',(28.3640892113951,2.9599971700504,1.7830513594197));
#32678=CARTESIAN_POINT('Ctrl Pts',(28.5198754062977,0.173103144446328,3.45046746880424));
#32679=CARTESIAN_POINT('Ctrl Pts',(28.6756616012002,-2.76896375813125,2.07058134389101));
#32680=CARTESIAN_POINT('Ctrl Pts',(28.8314477961028,-3.2589237700621,-1.14584557747595));
#32681=CARTESIAN_POINT('Ctrl Pts',(28.9353052593712,-1.671063172602,-2.60467617180897));
#32682=CARTESIAN_POINT('Ctrl Pts',(28.9872339910054,-0.742202251237312,
-2.84684032187586));
#32683=CARTESIAN_POINT('Ctrl Pts',(27.7778238829104,-2.9419205159921,0.00243417433800859));
#32684=CARTESIAN_POINT('Ctrl Pts',(27.8174594641694,-2.93560995158384,-0.730117559058909));
#32685=CARTESIAN_POINT('Ctrl Pts',(27.8570950454284,-2.65743809824621,-1.46695063553356));
#32686=CARTESIAN_POINT('Ctrl Pts',(27.8967306266874,-2.16167330950689,-2.00220524597985));
#32687=CARTESIAN_POINT('Ctrl Pts',(27.9486593583216,-1.5121448845319,-2.70347143506892));
#32688=CARTESIAN_POINT('Ctrl Pts',(28.0005880899558,-0.48911718900194,-3.05872726365523));
#32689=CARTESIAN_POINT('Ctrl Pts',(28.05251682159,0.455292944572102,-2.91104379138641));
#32690=CARTESIAN_POINT('Ctrl Pts',(28.1044455532242,1.39970307814614,-2.76336031911758));
#32691=CARTESIAN_POINT('Ctrl Pts',(28.1563742848584,2.26549564976426,-2.11273754599363));
#32692=CARTESIAN_POINT('Ctrl Pts',(28.2083030164925,2.66984342701799,-1.24656513738343));
#32693=CARTESIAN_POINT('Ctrl Pts',(28.2602317481267,3.07419120427171,-0.380392728773223));
#32694=CARTESIAN_POINT('Ctrl Pts',(28.3121604797609,3.01709418716105,0.701329315323246));
#32695=CARTESIAN_POINT('Ctrl Pts',(28.3640892113951,2.52406334100505,1.5200930222689));
#32696=CARTESIAN_POINT('Ctrl Pts',(28.4160179430293,2.03103249484904,2.33885672921455));
#32697=CARTESIAN_POINT('Ctrl Pts',(28.4679466746635,1.10206781964769,2.8946620990094));
#32698=CARTESIAN_POINT('Ctrl Pts',(28.5198754062977,0.147240998284077,2.94258376308795));
#32699=CARTESIAN_POINT('Ctrl Pts',(28.5659169375318,-0.699336369109807,
2.9850725111091));
#32700=CARTESIAN_POINT('Ctrl Pts',(28.6119584687659,-1.56624426411344,2.62830809441497));
#32701=CARTESIAN_POINT('Ctrl Pts',(28.658,-2.15060832247059,2.01293848078683));
#32702=CARTESIAN_POINT('',(22.6,-1.37977421736433,-1.93274596409627));
#32703=CARTESIAN_POINT('Ctrl Pts',(22.6,-1.3797742173643,-1.93274596409629));
#32704=CARTESIAN_POINT('Ctrl Pts',(22.6,-1.45785915848248,-1.89042312518908));
#32705=CARTESIAN_POINT('Ctrl Pts',(22.6,-1.53322062452788,-1.84365292533674));
#32706=CARTESIAN_POINT('Ctrl Pts',(22.6,-1.60541924836714,-1.7925389776215));
#32707=CARTESIAN_POINT('Ctrl Pts',(22.6,-1.67241398187154,-1.74510919124269));
#32708=CARTESIAN_POINT('Ctrl Pts',(22.6,-1.7366866559494,-1.6939390139514));
#32709=CARTESIAN_POINT('Ctrl Pts',(22.6,-1.79815525154635,-1.63938025328375));
#32710=CARTESIAN_POINT('Ctrl Pts',(22.6,-1.82774669609185,-1.61311525527802));
#32711=CARTESIAN_POINT('Ctrl Pts',(22.6,-1.85668798139578,-1.58606421212228));
#32712=CARTESIAN_POINT('Ctrl Pts',(22.6,-1.88496801744573,-1.55826263172972));
#32713=CARTESIAN_POINT('Ctrl Pts',(22.6,-1.89694635740944,-1.54648694725456));
#32714=CARTESIAN_POINT('Ctrl Pts',(22.6,-1.90880042781439,-1.5345820572415));
#32715=CARTESIAN_POINT('Ctrl Pts',(22.6,-1.92052581822529,-1.52255500426732));
#32716=CARTESIAN_POINT('Ctrl Pts',(22.6,-1.98100733369979,-1.46051746307855));
#32717=CARTESIAN_POINT('Ctrl Pts',(22.6,-2.03809982501458,-1.39520173965758));
#32718=CARTESIAN_POINT('Ctrl Pts',(22.6,-2.09171700828083,-1.32701838041071));
#32719=CARTESIAN_POINT('Ctrl Pts',(22.6,-2.1386320436388,-1.2673579410697));
#32720=CARTESIAN_POINT('Ctrl Pts',(22.6,-2.18288620426214,-1.20550076877931));
#32721=CARTESIAN_POINT('Ctrl Pts',(22.6,-2.2244039533604,-1.14169175518862));
#32722=CARTESIAN_POINT('Ctrl Pts',(22.6,-2.23783832694396,-1.12104434184867));
#32723=CARTESIAN_POINT('Ctrl Pts',(22.6,-2.25098603704135,-1.10019236804426));
#32724=CARTESIAN_POINT('Ctrl Pts',(22.6,-2.26384407676917,-1.07914361174352));
#32725=CARTESIAN_POINT('Ctrl Pts',(22.6,-2.27218773624139,-1.06548494692332));
#32726=CARTESIAN_POINT('Ctrl Pts',(22.6,-2.28040941692772,-1.05174341628636));
#32727=CARTESIAN_POINT('Ctrl Pts',(22.6,-2.28850824287345,-1.03792109526511));
#32728=CARTESIAN_POINT('Ctrl Pts',(22.6,-2.29616515491831,-1.02485299168755));
#32729=CARTESIAN_POINT('Ctrl Pts',(22.6,-2.30370706889497,-1.01172150964882));
#32730=CARTESIAN_POINT('Ctrl Pts',(22.6,-2.31113313207215,-0.998529628944857));
#32731=CARTESIAN_POINT('Ctrl Pts',(22.6,-2.35454850211762,-0.921405267261768));
#32732=CARTESIAN_POINT('Ctrl Pts',(22.6,-2.39401201422954,-0.842210569585459));
#32733=CARTESIAN_POINT('Ctrl Pts',(22.6,-2.42943733388716,-0.761342915874085));
#32734=CARTESIAN_POINT('Ctrl Pts',(22.6,-2.4654696596441,-0.679089610331911));
#32735=CARTESIAN_POINT('Ctrl Pts',(22.6,-2.49732484174602,-0.595104806954469));
#32736=CARTESIAN_POINT('Ctrl Pts',(22.6,-2.52487773536222,-0.509765448181997));
#32737=CARTESIAN_POINT('Ctrl Pts',(22.6,-2.5477911896283,-0.438795788095903));
#32738=CARTESIAN_POINT('Ctrl Pts',(22.6,-2.56772877983649,-0.366888349531481));
#32739=CARTESIAN_POINT('Ctrl Pts',(22.6,-2.584596243196,-0.29424448490606));
#32740=CARTESIAN_POINT('Ctrl Pts',(22.6,-2.59737320524494,-0.239217366623705));
#32741=CARTESIAN_POINT('Ctrl Pts',(22.6,-2.60838815722427,-0.183767373190182));
#32742=CARTESIAN_POINT('Ctrl Pts',(22.6,-2.61759113070643,-0.127978661306516));
#32743=CARTESIAN_POINT('Ctrl Pts',(22.6,-2.62055993379334,-0.10998168452769));
#32744=CARTESIAN_POINT('Ctrl Pts',(22.6,-2.62334060149709,-0.0919452294264881));
#32745=CARTESIAN_POINT('Ctrl Pts',(22.6,-2.62592758353743,-0.0739000925197149));
#32746=CARTESIAN_POINT('Ctrl Pts',(22.6,-2.63907517339903,0.0178091096886118));
#32747=CARTESIAN_POINT('Ctrl Pts',(22.6,-2.6472471121531,0.109869403253201));
#32748=CARTESIAN_POINT('Ctrl Pts',(22.6,-2.65032406207316,0.201881873939519));
#32749=CARTESIAN_POINT('Ctrl Pts',(22.6,-2.65219778541207,0.257913307104163));
#32750=CARTESIAN_POINT('Ctrl Pts',(22.6,-2.65218137509575,0.31392768209111));
#32751=CARTESIAN_POINT('Ctrl Pts',(22.6,-2.65023961232845,0.369839531880199));
#32752=CARTESIAN_POINT('Ctrl Pts',(22.6,-2.64715170229902,0.458753978399962));
#32753=CARTESIAN_POINT('Ctrl Pts',(22.6,-2.63919767846306,0.547409055573125));
#32754=CARTESIAN_POINT('Ctrl Pts',(22.6,-2.62661803880194,0.635544464197247));
#32755=CARTESIAN_POINT('Ctrl Pts',(22.6,-2.61933835618759,0.686547340205912));
#32756=CARTESIAN_POINT('Ctrl Pts',(22.6,-2.61050866025619,0.737376353293362));
#32757=CARTESIAN_POINT('Ctrl Pts',(22.6,-2.60016776191173,0.787981456082562));
#32758=CARTESIAN_POINT('Ctrl Pts',(22.6,-2.59279172176412,0.824077475733204));
#32759=CARTESIAN_POINT('Ctrl Pts',(22.6,-2.58464669361773,0.860059579007281));
#32760=CARTESIAN_POINT('Ctrl Pts',(22.6,-2.57574507716278,0.89590945104691));
#32761=CARTESIAN_POINT('Ctrl Pts',(22.6,-2.57127738066237,0.913902401952185));
#32762=CARTESIAN_POINT('Ctrl Pts',(22.6,-2.56661787459572,0.93186607753393));
#32763=CARTESIAN_POINT('Ctrl Pts',(22.6,-2.56177566668955,0.949771012880901));
#32764=CARTESIAN_POINT('Ctrl Pts',(22.6,-2.53764385793422,1.03900271956145));
#32765=CARTESIAN_POINT('Ctrl Pts',(22.6,-2.50895036688515,1.1268980164437));
#32766=CARTESIAN_POINT('Ctrl Pts',(22.6,-2.47598817745618,1.21317777136431));
#32767=CARTESIAN_POINT('Ctrl Pts',(22.6,-2.44237927848392,1.30115031253083));
#32768=CARTESIAN_POINT('Ctrl Pts',(22.6,-2.40433237097439,1.38744407152828));
#32769=CARTESIAN_POINT('Ctrl Pts',(22.6,-2.36210248902159,1.47176631907844));
#32770=CARTESIAN_POINT('Ctrl Pts',(22.6,-2.31948372457195,1.55686506527479));
#32771=CARTESIAN_POINT('Ctrl Pts',(22.6,-2.27260430302385,1.63995668918587));
#32772=CARTESIAN_POINT('Ctrl Pts',(22.6,-2.22167394745056,1.72073099208815));
#32773=CARTESIAN_POINT('Ctrl Pts',(22.6,-2.19223469061933,1.76742093606628));
#32774=CARTESIAN_POINT('Ctrl Pts',(22.6,-2.16144099506218,1.81333638138652));
#32775=CARTESIAN_POINT('Ctrl Pts',(22.6,-2.12932608668005,1.85841425069895));
#32776=CARTESIAN_POINT('Ctrl Pts',(22.6,-2.12079367180918,1.8703907158936));
#32777=CARTESIAN_POINT('Ctrl Pts',(22.6,-2.11216640274186,1.88231016366305));
#32778=CARTESIAN_POINT('Ctrl Pts',(22.6,-2.10344999573137,1.89416438598333));
#32779=CARTESIAN_POINT('Ctrl Pts',(22.6,-2.04526246313966,1.97329882139703));
#32780=CARTESIAN_POINT('Ctrl Pts',(22.6,-1.98324704259764,2.04933980788021));
#32781=CARTESIAN_POINT('Ctrl Pts',(22.6,-1.91768170146715,2.12198257731611));
#32782=CARTESIAN_POINT('Ctrl Pts',(22.6,-1.85187599989106,2.19489165282361));
#32783=CARTESIAN_POINT('Ctrl Pts',(22.6,-1.78249390688884,2.26437844634467));
#32784=CARTESIAN_POINT('Ctrl Pts',(22.6,-1.70976591886189,2.33011999619848));
#32785=CARTESIAN_POINT('Ctrl Pts',(22.6,-1.6383437830326,2.39468113738593));
#32786=CARTESIAN_POINT('Ctrl Pts',(22.6,-1.56369429611566,2.4556310976278));
#32787=CARTESIAN_POINT('Ctrl Pts',(22.6,-1.48599424012912,2.51263744458325));
#32788=CARTESIAN_POINT('Ctrl Pts',(22.6,-1.42232605236629,2.55934900425396));
#32789=CARTESIAN_POINT('Ctrl Pts',(22.6,-1.35660875961811,2.60341242494992));
#32790=CARTESIAN_POINT('Ctrl Pts',(22.6,-1.2889218540532,2.64462557919719));
#32791=CARTESIAN_POINT('Ctrl Pts',(22.6,-1.37977421736433,-1.93274596409627));
#32792=CARTESIAN_POINT('Ctrl Pts',(22.6460415312341,-0.820114607772339,
-2.32621799111725));
#32793=CARTESIAN_POINT('Ctrl Pts',(22.7440117941024,0.758470214248948,-2.63300441946709));
#32794=CARTESIAN_POINT('Ctrl Pts',(22.8939107886049,2.62282735660906,-0.938746401795666));
#32795=CARTESIAN_POINT('Ctrl Pts',(23.0496969835074,2.24240074214882,1.65328021767869));
#32796=CARTESIAN_POINT('Ctrl Pts',(23.2054831784101,-0.120664916242889,
2.78308709983206));
#32797=CARTESIAN_POINT('Ctrl Pts',(23.3384474812092,-2.04637284554299,1.64780428239185));
#32798=CARTESIAN_POINT('Ctrl Pts',(23.4194830523742,-2.36721675552049,0.4345208105624));
#32799=CARTESIAN_POINT('Ctrl Pts',(23.448589891905,-2.36840991602323,-0.000688909241090621));
#32800=CARTESIAN_POINT('Origin',(20.751410108095,0.,0.));
#32801=CARTESIAN_POINT('',(22.6,1.37702479013099,-1.93106208855767));
#32802=CARTESIAN_POINT('Origin',(22.6,0.,0.));
#32803=CARTESIAN_POINT('Ctrl Pts',(22.6,1.37702479013099,-1.93106208855767));
#32804=CARTESIAN_POINT('Ctrl Pts',(22.6519287316342,2.00708756429044,-1.48176940941637));
#32805=CARTESIAN_POINT('Ctrl Pts',(22.7557861949026,2.78394698441521,0.0732939610565424));
#32806=CARTESIAN_POINT('Ctrl Pts',(22.9115723898052,1.49072073679854,2.35522227267116));
#32807=CARTESIAN_POINT('Ctrl Pts',(23.0673585847077,-1.12180215515894,2.54924688068182));
#32808=CARTESIAN_POINT('Ctrl Pts',(23.1806378241377,-2.29982848865418,1.05373094085366));
#32809=CARTESIAN_POINT('Ctrl Pts',(23.2419883319334,-2.37405316087506,0.142149343728729));
#32810=CARTESIAN_POINT('Ctrl Pts',(23.251410108095,-2.37286196769524,0.00195470876282933));
#32811=CARTESIAN_POINT('Ctrl Pts',(22.2707660089946,1.70810875200394,-2.39535560853238));
#32812=CARTESIAN_POINT('Ctrl Pts',(22.3226947406288,2.48966021466954,-1.83803756825254));
#32813=CARTESIAN_POINT('Ctrl Pts',(22.4265522038972,3.45330326895732,0.0909163417005736));
#32814=CARTESIAN_POINT('Ctrl Pts',(22.5823383987997,1.84914110157534,2.92149844047583));
#32815=CARTESIAN_POINT('Ctrl Pts',(22.7381245937023,-1.39152184693901,3.16217321512214));
#32816=CARTESIAN_POINT('Ctrl Pts',(22.8939107886049,-3.40111157958131,0.61097941560448));
#32817=CARTESIAN_POINT('Ctrl Pts',(23.0496969835074,-2.40453763108011,-2.4821247976462));
#32818=CARTESIAN_POINT('Ctrl Pts',(23.20548317841,0.717935917613371,-3.38007436426549));
#32819=CARTESIAN_POINT('Ctrl Pts',(23.3612693733126,3.20561661195163,-1.29044022490378));
#32820=CARTESIAN_POINT('Ctrl Pts',(23.5170555682152,2.85953730127257,1.94020224751747));
#32821=CARTESIAN_POINT('Ctrl Pts',(23.6728417631178,-0.0144571353508022,
3.45555077544684));
#32822=CARTESIAN_POINT('Ctrl Pts',(23.8286279580203,-2.87565481901962,1.91619064272704));
#32823=CARTESIAN_POINT('Ctrl Pts',(23.9844141529229,-3.19472973788386,-1.31714785559497));
#32824=CARTESIAN_POINT('Ctrl Pts',(24.1402003478254,-0.68960129470691,-3.38608793893899));
#32825=CARTESIAN_POINT('Ctrl Pts',(24.295986542728,2.42514506376899,-2.46167280242748));
#32826=CARTESIAN_POINT('Ctrl Pts',(24.4517727376306,3.39602022813617,0.638909893803412));
#32827=CARTESIAN_POINT('Ctrl Pts',(24.6075589325332,1.36475126187535,3.1746825598677));
#32828=CARTESIAN_POINT('Ctrl Pts',(24.7633451274357,-1.8729823282135,2.90397922983507));
#32829=CARTESIAN_POINT('Ctrl Pts',(24.9191313223383,-3.45496565954171,0.066104969237162));
#32830=CARTESIAN_POINT('Ctrl Pts',(25.0749175172409,-1.98269651417726,-2.83020700980001));
#32831=CARTESIAN_POINT('Ctrl Pts',(25.2307037121434,1.24231233299229,-3.22456472193239));
#32832=CARTESIAN_POINT('Ctrl Pts',(25.386489907046,3.36909452241581,-0.768348565760258));
#32833=CARTESIAN_POINT('Ctrl Pts',(25.5422761019486,2.51753595578361,2.36710163085886));
#32834=CARTESIAN_POINT('Ctrl Pts',(25.6980622968512,-0.559570150281514,
3.40999103012744));
#32835=CARTESIAN_POINT('Ctrl Pts',(25.8538484917537,-3.14200602880735,1.43838635303248));
#32836=CARTESIAN_POINT('Ctrl Pts',(26.0096346866563,-2.94685160234359,-1.80477788365644));
#32837=CARTESIAN_POINT('Ctrl Pts',(26.1654208815589,-0.146626626641186,
-3.45248588722292));
#32838=CARTESIAN_POINT('Ctrl Pts',(26.3212070764614,2.78321855442789,-2.04813325762921));
#32839=CARTESIAN_POINT('Ctrl Pts',(26.476993271364,3.25264875345603,1.16680560889585));
#32840=CARTESIAN_POINT('Ctrl Pts',(26.6327794662666,0.846676835470829,3.35026863144008));
#32841=CARTESIAN_POINT('Ctrl Pts',(26.7885656611691,-2.30776977335729,2.57203035539396));
#32842=CARTESIAN_POINT('Ctrl Pts',(26.9443518560717,-3.42211190186477,-0.479923642607166));
#32843=CARTESIAN_POINT('Ctrl Pts',(27.1001380509743,-1.51123330277005,-3.10762789310822));
#32844=CARTESIAN_POINT('Ctrl Pts',(27.2559242458769,1.73558010371673,-2.98811008398895));
#32845=CARTESIAN_POINT('Ctrl Pts',(27.4117104407794,3.44815415895054,-0.227093009036346));
#32846=CARTESIAN_POINT('Ctrl Pts',(27.567496635682,2.1124088583074,2.73476555708426));
#32847=CARTESIAN_POINT('Ctrl Pts',(27.7232828305846,-1.09057038322062,3.27887037392547));
#32848=CARTESIAN_POINT('Ctrl Pts',(27.8790690254871,-3.32980739272074,0.924731019136299));
#32849=CARTESIAN_POINT('Ctrl Pts',(28.0348552203897,-2.62476217261374,-2.24754963466227));
#32850=CARTESIAN_POINT('Ctrl Pts',(28.1906414152923,0.399298518841041,-3.4316516702305));
#32851=CARTESIAN_POINT('Ctrl Pts',(28.3464276101949,3.07298101041792,-1.5846967094207));
#32852=CARTESIAN_POINT('Ctrl Pts',(28.5022138050974,3.0248495908613,1.66848859787707));
#32853=CARTESIAN_POINT('Ctrl Pts',(28.6060712683658,1.21780515048259,2.84495003511031));
#32854=CARTESIAN_POINT('Ctrl Pts',(28.658,0.261701021631923,2.93033728012268));
#32855=CARTESIAN_POINT('Ctrl Pts',(22.3805106726631,1.59774743137962,-2.24059110187414));
#32856=CARTESIAN_POINT('Ctrl Pts',(22.4324394042973,2.32880266454317,-1.71928151530715));
#32857=CARTESIAN_POINT('Ctrl Pts',(22.5362968675656,3.23018450744328,0.0850422148192308));
#32858=CARTESIAN_POINT('Ctrl Pts',(22.6920830624682,1.72966764664974,2.73273971787427));
#32859=CARTESIAN_POINT('Ctrl Pts',(22.8478692573708,-1.30161528301232,2.95786443697537));
#32860=CARTESIAN_POINT('Ctrl Pts',(23.0036554522734,-3.18136493577254,0.571503887420878));
#32861=CARTESIAN_POINT('Ctrl Pts',(23.1594416471759,-2.24917987171874,-2.32175411264079));
#32862=CARTESIAN_POINT('Ctrl Pts',(23.3152278420785,0.671549903901719,-3.16168694003907));
#32863=CARTESIAN_POINT('Ctrl Pts',(23.471014036981,2.99850094540219,-1.20706456908558));
#32864=CARTESIAN_POINT('Ctrl Pts',(23.6268002318837,2.67478190289836,1.81484530987337));
#32865=CARTESIAN_POINT('Ctrl Pts',(23.7825864267862,-0.0135230563304296,
3.23228680199357));
#32866=CARTESIAN_POINT('Ctrl Pts',(23.9383726216888,-2.68985806391585,1.79238510069044));
#32867=CARTESIAN_POINT('Ctrl Pts',(24.0941588165913,-2.98831747490762,-1.23204661328215));
#32868=CARTESIAN_POINT('Ctrl Pts',(24.2499450114939,-0.645045987851415,
-3.16731197619483));
#32869=CARTESIAN_POINT('Ctrl Pts',(24.4057312063965,2.26845585318501,-2.30262352579206));
#32870=CARTESIAN_POINT('Ctrl Pts',(24.561517401299,3.17660253777874,0.597629770651206));
#32871=CARTESIAN_POINT('Ctrl Pts',(24.7173035962016,1.27657435194057,2.96956554992383));
#32872=CARTESIAN_POINT('Ctrl Pts',(24.8730897911042,-1.75196848585414,2.71635242768082));
#32873=CARTESIAN_POINT('Ctrl Pts',(25.0288759860068,-3.23173949056894,0.0618339111465752));
#32874=CARTESIAN_POINT('Ctrl Pts',(25.1846621809093,-1.85459401166088,-2.64734664866943));
#32875=CARTESIAN_POINT('Ctrl Pts',(25.3404483758119,1.16204623193985,-3.01622481340282));
#32876=CARTESIAN_POINT('Ctrl Pts',(25.4962345707145,3.15141650843352,-0.718705378628512));
#32877=CARTESIAN_POINT('Ctrl Pts',(25.6520207656171,2.35487734726496,2.21416262054873));
#32878=CARTESIAN_POINT('Ctrl Pts',(25.8078069605196,-0.523416187195402,
3.18967068286592));
#32879=CARTESIAN_POINT('Ctrl Pts',(25.9635931554222,-2.93900025745823,1.34545186200406));
#32880=CARTESIAN_POINT('Ctrl Pts',(26.1193793503248,-2.75645480580648,-1.68817074699713));
#32881=CARTESIAN_POINT('Ctrl Pts',(26.2751655452273,-0.137153044742009,
-3.22941993694093));
#32882=CARTESIAN_POINT('Ctrl Pts',(26.4309517401299,2.60339412879199,-1.91580287125224));
#32883=CARTESIAN_POINT('Ctrl Pts',(26.5867379350325,3.04249432884032,1.09141801559505));
#32884=CARTESIAN_POINT('Ctrl Pts',(26.7425241299351,0.791972839841186,3.13380696283837));
#32885=CARTESIAN_POINT('Ctrl Pts',(26.8983103248376,-2.15866420874626,2.40585085050347));
#32886=CARTESIAN_POINT('Ctrl Pts',(27.0540965197402,-3.20100842214141,-0.448915659693424));
#32887=CARTESIAN_POINT('Ctrl Pts',(27.2098827146427,-1.41359215265622,-2.90684330144212));
#32888=CARTESIAN_POINT('Ctrl Pts',(27.3656689095453,1.6234438523974,-2.79504756694899));
#32889=CARTESIAN_POINT('Ctrl Pts',(27.5214551044479,3.22536808268251,-0.212420474660298));
#32890=CARTESIAN_POINT('Ctrl Pts',(27.6772412993505,1.97592560978601,2.5580716913549));
#32891=CARTESIAN_POINT('Ctrl Pts',(27.833027494253,-1.0201083663351,3.06702176405338));
#32892=CARTESIAN_POINT('Ctrl Pts',(27.9888136891556,-3.11466772971383,0.864983923774584));
#32893=CARTESIAN_POINT('Ctrl Pts',(28.1445998840582,-2.45517565222704,-2.10233490781362));
#32894=CARTESIAN_POINT('Ctrl Pts',(28.3003860789607,0.373499744722629,-3.20993182375997));
#32895=CARTESIAN_POINT('Ctrl Pts',(28.4561722738633,2.87443496224312,-1.48230907079083));
#32896=CARTESIAN_POINT('Ctrl Pts',(28.6119584687659,2.82941332537425,1.56068714501741));
#32897=CARTESIAN_POINT('Ctrl Pts',(28.7158159320343,1.13912246443424,2.66113712353977));
#32898=CARTESIAN_POINT('Ctrl Pts',(28.7677446636685,0.244792455170829,2.74100747794843));
#32899=CARTESIAN_POINT('Ctrl Pts',(22.4902553363315,1.4873861107553,-2.08582659521591));
#32900=CARTESIAN_POINT('Ctrl Pts',(22.5421840679657,2.16794511441681,-1.60052546236176));
#32901=CARTESIAN_POINT('Ctrl Pts',(22.6460415312341,3.00706574592924,0.0791680879378876));
#32902=CARTESIAN_POINT('Ctrl Pts',(22.8018277261367,1.61019419172414,2.54398099527271));
#32903=CARTESIAN_POINT('Ctrl Pts',(22.9576139210392,-1.21170871908563,2.7535556588286));
#32904=CARTESIAN_POINT('Ctrl Pts',(23.1134001159418,-2.96161829196376,0.532028359237276));
#32905=CARTESIAN_POINT('Ctrl Pts',(23.2691863108444,-2.09382211235737,-2.16138342763538));
#32906=CARTESIAN_POINT('Ctrl Pts',(23.4249725057469,0.625163890190072,-2.94329951581265));
#32907=CARTESIAN_POINT('Ctrl Pts',(23.5807587006496,2.79138527885274,-1.12368891326739));
#32908=CARTESIAN_POINT('Ctrl Pts',(23.7365448955521,2.49002650452417,1.68948837222927));
#32909=CARTESIAN_POINT('Ctrl Pts',(23.8923310904547,-0.0125889773100609,
3.0090228285403));
#32910=CARTESIAN_POINT('Ctrl Pts',(24.0481172853572,-2.50406130881207,1.66857955865383));
#32911=CARTESIAN_POINT('Ctrl Pts',(24.2039034802599,-2.78190521193138,-1.14694537096932));
#32912=CARTESIAN_POINT('Ctrl Pts',(24.3596896751623,-0.600490680995917,
-2.94853601345067));
#32913=CARTESIAN_POINT('Ctrl Pts',(24.515475870065,2.11176664260102,-2.14357424915663));
#32914=CARTESIAN_POINT('Ctrl Pts',(24.6712620649675,2.95718484742131,0.556349647498999));
#32915=CARTESIAN_POINT('Ctrl Pts',(24.8270482598701,1.18839744200578,2.76444853997997));
#32916=CARTESIAN_POINT('Ctrl Pts',(24.9828344547727,-1.63095464349477,2.52872562552656));
#32917=CARTESIAN_POINT('Ctrl Pts',(25.1386206496752,-3.00851332159618,0.0575628530559896));
#32918=CARTESIAN_POINT('Ctrl Pts',(25.2944068445778,-1.7264915091445,-2.46448628753886));
#32919=CARTESIAN_POINT('Ctrl Pts',(25.4501930394804,1.08178013088741,-2.80788490487326));
#32920=CARTESIAN_POINT('Ctrl Pts',(25.6059792343829,2.93373849445125,-0.669062191496764));
#32921=CARTESIAN_POINT('Ctrl Pts',(25.7617654292855,2.19221873874631,2.06122361023859));
#32922=CARTESIAN_POINT('Ctrl Pts',(25.9175516241881,-0.48726222410929,2.9693503356044));
#32923=CARTESIAN_POINT('Ctrl Pts',(26.0733378190906,-2.7359944861091,1.25251737097565));
#32924=CARTESIAN_POINT('Ctrl Pts',(26.2291240139933,-2.56605800926939,-1.57156361033782));
#32925=CARTESIAN_POINT('Ctrl Pts',(26.3849102088958,-0.127679462842828,
-3.00635398665893));
#32926=CARTESIAN_POINT('Ctrl Pts',(26.5406964037984,2.42356970315608,-1.78347248487528));
#32927=CARTESIAN_POINT('Ctrl Pts',(26.6964825987009,2.8323399042246,1.01603042229426));
#32928=CARTESIAN_POINT('Ctrl Pts',(26.8522687936035,0.737268844211538,2.91734529423666));
#32929=CARTESIAN_POINT('Ctrl Pts',(27.0080549885061,-2.00955864413522,2.23967134561299));
#32930=CARTESIAN_POINT('Ctrl Pts',(27.1638411834087,-2.97990494241805,-0.417907676779675));
#32931=CARTESIAN_POINT('Ctrl Pts',(27.3196273783112,-1.3159510025424,-2.70605870977603));
#32932=CARTESIAN_POINT('Ctrl Pts',(27.4754135732138,1.51130760107806,-2.60198504990902));
#32933=CARTESIAN_POINT('Ctrl Pts',(27.6311997681163,3.0025820064145,-0.197747940284252));
#32934=CARTESIAN_POINT('Ctrl Pts',(27.7869859630189,1.83944236126462,2.38137782562555));
#32935=CARTESIAN_POINT('Ctrl Pts',(27.9427721579215,-0.949646349449587,
2.8551731541813));
#32936=CARTESIAN_POINT('Ctrl Pts',(28.0985583528241,-2.89952806670692,0.805236828412871));
#32937=CARTESIAN_POINT('Ctrl Pts',(28.2543445477266,-2.28558913184034,-1.95712018096498));
#32938=CARTESIAN_POINT('Ctrl Pts',(28.4101307426292,0.347700970604219,-2.98821197728943));
#32939=CARTESIAN_POINT('Ctrl Pts',(28.5659169375318,2.67588891406832,-1.37992143216097));
#32940=CARTESIAN_POINT('Ctrl Pts',(28.7217031324344,2.6339770598872,1.45288569215775));
#32941=CARTESIAN_POINT('Ctrl Pts',(28.8255605957027,1.06043977838589,2.47732421196922));
#32942=CARTESIAN_POINT('Ctrl Pts',(28.8774893273369,0.227883888709735,2.55167767577418));
#32943=CARTESIAN_POINT('Ctrl Pts',(22.6,1.37702479013099,-1.93106208855767));
#32944=CARTESIAN_POINT('Ctrl Pts',(22.6519287316342,2.00708756429044,-1.48176940941637));
#32945=CARTESIAN_POINT('Ctrl Pts',(22.7557861949026,2.78394698441521,0.0732939610565424));
#32946=CARTESIAN_POINT('Ctrl Pts',(22.9115723898052,1.49072073679854,2.35522227267116));
#32947=CARTESIAN_POINT('Ctrl Pts',(23.0673585847077,-1.12180215515894,2.54924688068182));
#32948=CARTESIAN_POINT('Ctrl Pts',(23.2231447796103,-2.74187164815499,0.492552831053676));
#32949=CARTESIAN_POINT('Ctrl Pts',(23.3789309745128,-1.938464352996,-2.00101274262997));
#32950=CARTESIAN_POINT('Ctrl Pts',(23.5347171694154,0.578777876478422,-2.72491209158622));
#32951=CARTESIAN_POINT('Ctrl Pts',(23.690503364318,2.58426961230329,-1.04031325744919));
#32952=CARTESIAN_POINT('Ctrl Pts',(23.8462895592206,2.30527110614996,1.56413143458517));
#32953=CARTESIAN_POINT('Ctrl Pts',(24.0020757541231,-0.0116548982896913,
2.78575885508703));
#32954=CARTESIAN_POINT('Ctrl Pts',(24.1578619490257,-2.3182645537083,1.54477401661722));
#32955=CARTESIAN_POINT('Ctrl Pts',(24.3136481439283,-2.57549294895514,-1.06184412865649));
#32956=CARTESIAN_POINT('Ctrl Pts',(24.4694343388309,-0.555935374140417,
-2.72976005070651));
#32957=CARTESIAN_POINT('Ctrl Pts',(24.6252205337334,1.95507743201704,-1.9845249725212));
#32958=CARTESIAN_POINT('Ctrl Pts',(24.781006728636,2.73776715706389,0.51506952434679));
#32959=CARTESIAN_POINT('Ctrl Pts',(24.9367929235385,1.10022053207099,2.55933153003611));
#32960=CARTESIAN_POINT('Ctrl Pts',(25.0925791184411,-1.50994080113541,2.3410988233723));
#32961=CARTESIAN_POINT('Ctrl Pts',(25.2483653133437,-2.7852871526234,0.0532917949654058));
#32962=CARTESIAN_POINT('Ctrl Pts',(25.4041515082462,-1.59838900662812,-2.28162592640829));
#32963=CARTESIAN_POINT('Ctrl Pts',(25.5599377031489,1.00151402983497,-2.59954499634369));
#32964=CARTESIAN_POINT('Ctrl Pts',(25.7157238980514,2.71606048046896,-0.619419004365017));
#32965=CARTESIAN_POINT('Ctrl Pts',(25.871510092954,2.02956013022766,1.90828459992846));
#32966=CARTESIAN_POINT('Ctrl Pts',(26.0272962878565,-0.451108261023179,
2.74902998834288));
#32967=CARTESIAN_POINT('Ctrl Pts',(26.1830824827591,-2.53298871475997,1.15958287994724));
#32968=CARTESIAN_POINT('Ctrl Pts',(26.3388686776617,-2.37566121273229,-1.45495647367851));
#32969=CARTESIAN_POINT('Ctrl Pts',(26.4946548725642,-0.118205880943649,
-2.78328803637694));
#32970=CARTESIAN_POINT('Ctrl Pts',(26.6504410674669,2.24374527752018,-1.65114209849832));
#32971=CARTESIAN_POINT('Ctrl Pts',(26.8062272623694,2.62218547960889,0.940642828993458));
#32972=CARTESIAN_POINT('Ctrl Pts',(26.962013457272,0.682564848581893,2.70088362563495));
#32973=CARTESIAN_POINT('Ctrl Pts',(27.1177996521745,-1.86045307952419,2.07349184072251));
#32974=CARTESIAN_POINT('Ctrl Pts',(27.2735858470771,-2.75880146269469,-0.386899693865931));
#32975=CARTESIAN_POINT('Ctrl Pts',(27.4293720419797,-1.21830985242857,-2.50527411810993));
#32976=CARTESIAN_POINT('Ctrl Pts',(27.5851582368822,1.39917134975873,-2.40892253286906));
#32977=CARTESIAN_POINT('Ctrl Pts',(27.7409444317848,2.77979593014647,-0.183075405908203));
#32978=CARTESIAN_POINT('Ctrl Pts',(27.8967306266874,1.70295911274323,2.20468395989619));
#32979=CARTESIAN_POINT('Ctrl Pts',(28.05251682159,-0.879184332564077,2.64332454430922));
#32980=CARTESIAN_POINT('Ctrl Pts',(28.2083030164925,-2.6843884037,0.745489733051156));
#32981=CARTESIAN_POINT('Ctrl Pts',(28.3640892113951,-2.11600261145364,-1.81190545411633));
#32982=CARTESIAN_POINT('Ctrl Pts',(28.5198754062977,0.321902196485808,-2.7664921308189));
#32983=CARTESIAN_POINT('Ctrl Pts',(28.6756616012002,2.47734286589352,-1.27753379353111));
#32984=CARTESIAN_POINT('Ctrl Pts',(28.8314477961028,2.43854079440016,1.34508423929808));
#32985=CARTESIAN_POINT('Ctrl Pts',(28.9353052593712,0.981757092337547,2.29351130039867));
#32986=CARTESIAN_POINT('Ctrl Pts',(28.9872339910054,0.210975322248641,2.36234787359992));
#32987=CARTESIAN_POINT('Ctrl Pts',(22.6,1.29193968544099,2.64724960214528));
#32988=CARTESIAN_POINT('Ctrl Pts',(22.6,1.37398662210897,2.59799179582031));
#32989=CARTESIAN_POINT('Ctrl Pts',(22.6,1.45331123519463,2.54465519870452));
#32990=CARTESIAN_POINT('Ctrl Pts',(22.6,1.52954787739396,2.48723802283488));
#32991=CARTESIAN_POINT('Ctrl Pts',(22.6,1.53975420128136,2.4795511904047));
#32992=CARTESIAN_POINT('Ctrl Pts',(22.6,1.54990512670829,2.471791166031));
#32993=CARTESIAN_POINT('Ctrl Pts',(22.6,1.55999972524662,2.46395789450524));
#32994=CARTESIAN_POINT('Ctrl Pts',(22.6,1.63744923949508,2.4038581221029));
#32995=CARTESIAN_POINT('Ctrl Pts',(22.6,1.71158671352519,2.33944889993133));
#32996=CARTESIAN_POINT('Ctrl Pts',(22.6,1.7822309969812,2.27110880309472));
#32997=CARTESIAN_POINT('Ctrl Pts',(22.6,1.80301535614779,2.25100236208289));
#32998=CARTESIAN_POINT('Ctrl Pts',(22.6,1.82349704371371,2.23055549420075));
#32999=CARTESIAN_POINT('Ctrl Pts',(22.6,1.84367067623173,2.20977747618807));
#33000=CARTESIAN_POINT('Ctrl Pts',(22.6,1.85694131862264,2.19610925622859));
#33001=CARTESIAN_POINT('Ctrl Pts',(22.6,1.87007864940316,2.18229773526248));
#33002=CARTESIAN_POINT('Ctrl Pts',(22.6,1.88308104907989,2.16834552726226));
#33003=CARTESIAN_POINT('Ctrl Pts',(22.6,1.89645232297084,2.15399749926799));
#33004=CARTESIAN_POINT('Ctrl Pts',(22.6,1.90967535655003,2.13950656026653));
#33005=CARTESIAN_POINT('Ctrl Pts',(22.6,1.92274364758183,2.12488175434569));
#33006=CARTESIAN_POINT('Ctrl Pts',(22.6,1.98743002993418,2.0524908208011));
#33007=CARTESIAN_POINT('Ctrl Pts',(22.6,2.04837002339202,1.97677788797286));
#33008=CARTESIAN_POINT('Ctrl Pts',(22.6,2.10540137231736,1.89812284077031));
#33009=CARTESIAN_POINT('Ctrl Pts',(22.6,2.15306292861443,1.83239018617011));
#33010=CARTESIAN_POINT('Ctrl Pts',(22.6,2.19799397733902,1.76460187700287));
#33011=CARTESIAN_POINT('Ctrl Pts',(22.6,2.24007370157356,1.69496974001289));
#33012=CARTESIAN_POINT('Ctrl Pts',(22.6,2.2588040734674,1.66397533961436));
#33013=CARTESIAN_POINT('Ctrl Pts',(22.6,2.27696918818612,1.63261554623335));
#33014=CARTESIAN_POINT('Ctrl Pts',(22.6,2.2945567623349,1.60090880756888));
#33015=CARTESIAN_POINT('Ctrl Pts',(22.6,2.30328860155935,1.58516711732737));
#33016=CARTESIAN_POINT('Ctrl Pts',(22.6,2.31187806677236,1.56933990751256));
#33017=CARTESIAN_POINT('Ctrl Pts',(22.6,2.32032355901159,1.55342943411423));
#33018=CARTESIAN_POINT('Ctrl Pts',(22.6,2.32804618004994,1.53888077867587));
#33019=CARTESIAN_POINT('Ctrl Pts',(22.6,2.33564454313757,1.52426973302578));
#33020=CARTESIAN_POINT('Ctrl Pts',(22.6,2.34311514756603,1.50960353912746));
#33021=CARTESIAN_POINT('Ctrl Pts',(22.6,2.3862343690969,1.42495244164634));
#33022=CARTESIAN_POINT('Ctrl Pts',(22.6,2.42513144916236,1.33840899559929));
#33023=CARTESIAN_POINT('Ctrl Pts',(22.6,2.45965235719831,1.25032466278114));
#33024=CARTESIAN_POINT('Ctrl Pts',(22.6,2.49387162064543,1.16301001314535));
#33025=CARTESIAN_POINT('Ctrl Pts',(22.6,2.52379105451494,1.07418035409301));
#33026=CARTESIAN_POINT('Ctrl Pts',(22.6,2.54921046539056,0.98416944937067));
#33027=CARTESIAN_POINT('Ctrl Pts',(22.6,2.57014848001453,0.910027304668119));
#33028=CARTESIAN_POINT('Ctrl Pts',(22.6,2.58803245793096,0.83508332520754));
#33029=CARTESIAN_POINT('Ctrl Pts',(22.6,2.60272312322177,0.759526199301805));
#33030=CARTESIAN_POINT('Ctrl Pts',(22.6,2.61374112218987,0.702858354872504));
#33031=CARTESIAN_POINT('Ctrl Pts',(22.6,2.62296238253348,0.645845632245045));
#33032=CARTESIAN_POINT('Ctrl Pts',(22.6,2.63031846040409,0.588570176538994));
#33033=CARTESIAN_POINT('Ctrl Pts',(22.6,2.63217022162964,0.574152103495507));
#33034=CARTESIAN_POINT('Ctrl Pts',(22.6,2.63390374573031,0.559717395949854));
#33035=CARTESIAN_POINT('Ctrl Pts',(22.6,2.63551785486944,0.545267396301203));
#33036=CARTESIAN_POINT('Ctrl Pts',(22.6,2.63700943918069,0.531914276458778));
#33037=CARTESIAN_POINT('Ctrl Pts',(22.6,2.63839851735333,0.518552496504733));
#33038=CARTESIAN_POINT('Ctrl Pts',(22.6,2.63968370751675,0.505190950925346));
#33039=CARTESIAN_POINT('Ctrl Pts',(22.6,2.64822927439902,0.416346525680822));
#33040=CARTESIAN_POINT('Ctrl Pts',(22.6,2.65219771421662,0.327406838635517));
#33041=CARTESIAN_POINT('Ctrl Pts',(22.6,2.65141649101387,0.238668286707819));
#33042=CARTESIAN_POINT('Ctrl Pts',(22.6,2.65092714796485,0.183084180382702));
#33043=CARTESIAN_POINT('Ctrl Pts',(22.6,2.64857327480457,0.127578997259634));
#33044=CARTESIAN_POINT('Ctrl Pts',(22.6,2.6443021234377,0.0722273116339143));
#33045=CARTESIAN_POINT('Ctrl Pts',(22.6,2.63733327280372,-0.018085017836793));
#33046=CARTESIAN_POINT('Ctrl Pts',(22.6,2.6252624315387,-0.107990203752847));
#33047=CARTESIAN_POINT('Ctrl Pts',(22.6,2.60828201361834,-0.197151736827924));
#33048=CARTESIAN_POINT('Ctrl Pts',(22.6,2.59124313592887,-0.28662023305671));
#33049=CARTESIAN_POINT('Ctrl Pts',(22.6,2.56926019798414,-0.375340802433049));
#33050=CARTESIAN_POINT('Ctrl Pts',(22.6,2.54248600040002,-0.462941832765398));
#33051=CARTESIAN_POINT('Ctrl Pts',(22.6,2.53837999571101,-0.476376044572389));
#33052=CARTESIAN_POINT('Ctrl Pts',(22.6,2.53416363894075,-0.489775921708853));
#33053=CARTESIAN_POINT('Ctrl Pts',(22.6,2.5298392091435,-0.503136034212508));
#33054=CARTESIAN_POINT('Ctrl Pts',(22.6,2.50253277200761,-0.587497924522625));
#33055=CARTESIAN_POINT('Ctrl Pts',(22.6,2.47090442181699,-0.670330946599523));
#33056=CARTESIAN_POINT('Ctrl Pts',(22.6,2.43517017876197,-0.751334282795894));
#33057=CARTESIAN_POINT('Ctrl Pts',(22.6,2.39947016711518,-0.83226002232216));
#33058=CARTESIAN_POINT('Ctrl Pts',(22.6,2.35967146038532,-0.911360358667436));
#33059=CARTESIAN_POINT('Ctrl Pts',(22.6,2.31594727372697,-0.988305313713532));
#33060=CARTESIAN_POINT('Ctrl Pts',(22.6,2.2729032797118,-1.06405327925901));
#33061=CARTESIAN_POINT('Ctrl Pts',(22.6,2.22605430689985,-1.137713018672));
#33062=CARTESIAN_POINT('Ctrl Pts',(22.6,2.17553481696067,-1.20893040656016));
#33063=CARTESIAN_POINT('Ctrl Pts',(22.6,2.15829884607901,-1.23322797617905));
#33064=CARTESIAN_POINT('Ctrl Pts',(22.6,2.14063540467206,-1.25724087327014));
#33065=CARTESIAN_POINT('Ctrl Pts',(22.6,2.12254920670209,-1.28095377076072));
#33066=CARTESIAN_POINT('Ctrl Pts',(22.6,2.11108446021501,-1.29598525270375));
#33067=CARTESIAN_POINT('Ctrl Pts',(22.6,2.09944983480608,-1.3108961744379));
#33068=CARTESIAN_POINT('Ctrl Pts',(22.6,2.08764647715969,-1.32568248351855));
#33069=CARTESIAN_POINT('Ctrl Pts',(22.6,2.07921581304034,-1.33624374999529));
#33070=CARTESIAN_POINT('Ctrl Pts',(22.6,2.07070458118542,-1.34673450751064));
#33071=CARTESIAN_POINT('Ctrl Pts',(22.6,2.06211537646975,-1.35715132281721));
#33072=CARTESIAN_POINT('Ctrl Pts',(22.6,2.007856874164,-1.42295494678941));
#33073=CARTESIAN_POINT('Ctrl Pts',(22.6,1.95046520729726,-1.48584152571506));
#33074=CARTESIAN_POINT('Ctrl Pts',(22.6,1.89010219144091,-1.54551632835672));
#33075=CARTESIAN_POINT('Ctrl Pts',(22.6,1.83067278976528,-1.60426816117674));
#33076=CARTESIAN_POINT('Ctrl Pts',(22.6,1.76836259681773,-1.65990731572679));
#33077=CARTESIAN_POINT('Ctrl Pts',(22.6,1.70330015578668,-1.71211004597693));
#33078=CARTESIAN_POINT('Ctrl Pts',(22.6,1.64025601666085,-1.76269339539456));
#33079=CARTESIAN_POINT('Ctrl Pts',(22.6,1.57462716209707,-1.81005050265833));
#33080=CARTESIAN_POINT('Ctrl Pts',(22.6,1.50651496632111,-1.85384102298016));
#33081=CARTESIAN_POINT('Ctrl Pts',(22.6,1.46429839471039,-1.88098279422944));
#33082=CARTESIAN_POINT('Ctrl Pts',(22.6,1.42112754045947,-1.90675349235672));
#33083=CARTESIAN_POINT('Ctrl Pts',(22.6,1.37702479013099,-1.93106208855767));
#33084=CARTESIAN_POINT('Ctrl Pts',(28.658,0.261701021631923,2.93033728012268));
#33085=CARTESIAN_POINT('Ctrl Pts',(28.6060712683658,1.21780515048259,2.84495003511031));
#33086=CARTESIAN_POINT('Ctrl Pts',(28.5541425367316,2.12132737067194,2.25671931649369));
#33087=CARTESIAN_POINT('Ctrl Pts',(28.5022138050974,2.58111038402606,1.42040640596909));
#33088=CARTESIAN_POINT('Ctrl Pts',(28.4502850734632,3.04089339738017,0.584093495444484));
#33089=CARTESIAN_POINT('Ctrl Pts',(28.3983563418291,3.05693720389905,-0.500301606988106));
#33090=CARTESIAN_POINT('Ctrl Pts',(28.3464276101949,2.61934535856234,-1.35032498500603));
#33091=CARTESIAN_POINT('Ctrl Pts',(28.2944988785607,2.18175351322563,-2.20034836302396));
#33092=CARTESIAN_POINT('Ctrl Pts',(28.2425701469265,1.29052601603334,-2.81600001662723));
#33093=CARTESIAN_POINT('Ctrl Pts',(28.1906414152923,0.340902152194731,-2.9264755041675));
#33094=CARTESIAN_POINT('Ctrl Pts',(28.1387126836581,-0.608721711643891,
-3.03695099170776));
#33095=CARTESIAN_POINT('Ctrl Pts',(28.0867839520239,-1.61674194212883,-2.64225031318501));
#33096=CARTESIAN_POINT('Ctrl Pts',(28.0348552203897,-2.23825959405579,-1.91618653162386));
#33097=CARTESIAN_POINT('Ctrl Pts',(27.9972955192897,-2.68779911678517,-1.39102949896014));
#33098=CARTESIAN_POINT('Ctrl Pts',(27.9597358181896,-2.93513860722871,-0.692518823009792));
#33099=CARTESIAN_POINT('Ctrl Pts',(27.9221761170896,-2.94084529159276,0.00236346891266642));
#33100=CARTESIAN_POINT('Origin',(25.6,0.,0.));
#33101=CARTESIAN_POINT('Origin',(28.658,0.,0.));
#33102=CARTESIAN_POINT('Origin',(2.,4.6,0.));
#33103=CARTESIAN_POINT('',(2.,-4.6,-5.63337527607782E-16));
#33104=CARTESIAN_POINT('Origin',(2.,0.,0.));
#33105=CARTESIAN_POINT('Origin',(2.2,0.,0.));
#33106=CARTESIAN_POINT('',(2.4,-5.,-6.12323399573676E-16));
#33107=CARTESIAN_POINT('Origin',(2.4,0.,0.));
#33108=CARTESIAN_POINT('',(2.2,-4.8,-5.87830463590729E-16));
#33109=CARTESIAN_POINT('Origin',(12.5,0.,0.));
#33110=CARTESIAN_POINT('',(22.6,-5.,-6.12323399573677E-16));
#33111=CARTESIAN_POINT('Origin',(22.6,0.,0.));
#33112=CARTESIAN_POINT('',(12.5,-5.,-6.12323399573677E-16));
#33113=CARTESIAN_POINT('Origin',(22.6,3.,0.));
#33114=CARTESIAN_POINT('Origin',(28.8,0.,0.));
#33115=CARTESIAN_POINT('',(29.,-2.6,-3.18408167778312E-16));
#33116=CARTESIAN_POINT('Origin',(29.,0.,0.));
#33117=CARTESIAN_POINT('',(28.8,-2.8,-3.42901103761259E-16));
#33118=CARTESIAN_POINT('Origin',(29.,0.,0.));
#33119=CARTESIAN_POINT('',(0.,0.,0.));
#33120=CARTESIAN_POINT('Origin',(8.51525479982404,0.,-5.85844879599047E-16));
#33121=CARTESIAN_POINT('',(8.63975534938695,9.2422018555175,-1.13184329194332E-15));
#33122=CARTESIAN_POINT('',(8.63975534938694,-9.2422018555175,-1.13184329194332E-15));
#33123=CARTESIAN_POINT('Origin',(8.63975534938695,0.,-5.65921645971662E-16));
#33124=CARTESIAN_POINT('Origin',(8.63975534938695,0.,-5.65921645971662E-16));
#33125=CARTESIAN_POINT('',(8.39075425026112,9.89294404963443,1.21153622645287E-15));
#33126=CARTESIAN_POINT('',(8.51525479982404,9.56757295257596,1.17168975919809E-15));
#33127=CARTESIAN_POINT('',(8.39075425026113,-9.89294404963442,-1.21153622645287E-15));
#33128=CARTESIAN_POINT('Origin',(8.39075425026112,0.,-6.05768113226433E-16));
#33129=CARTESIAN_POINT('Origin',(8.39075425026112,0.,-6.05768113226433E-16));
#33130=CARTESIAN_POINT('Origin',(8.1,0.,0.));
#33131=CARTESIAN_POINT('',(7.6,-11.,-1.34711147906209E-15));
#33132=CARTESIAN_POINT('',(8.1,-10.3,-1.26138620312177E-15));
#33133=CARTESIAN_POINT('Origin',(7.6,0.,0.));
#33134=CARTESIAN_POINT('Origin',(8.8,0.,0.));
#33135=CARTESIAN_POINT('',(9.,-6.,-7.34788079488412E-16));
#33136=CARTESIAN_POINT('Origin',(9.,0.,0.));
#33137=CARTESIAN_POINT('',(8.8,-7.8,-9.55224503334935E-16));
#33138=CARTESIAN_POINT('Origin',(8.7,5.6,0.));
#33139=CARTESIAN_POINT('',(8.7,-5.6,-6.85802207522518E-16));
#33140=CARTESIAN_POINT('Origin',(8.7,0.,0.));
#33141=CARTESIAN_POINT('',(8.7,-5.,-6.12323399573677E-16));
#33142=CARTESIAN_POINT('Origin',(8.7,0.,0.));
#33143=CARTESIAN_POINT('Origin',(8.855,0.,0.));
#33144=CARTESIAN_POINT('',(9.,-5.6,6.85802207522518E-16));
#33145=CARTESIAN_POINT('',(8.855,-5.6,-6.85802207522518E-16));
#33146=CARTESIAN_POINT('Origin',(9.,0.,0.));
#33147=CARTESIAN_POINT('Origin',(8.855,0.,0.));
#33148=CARTESIAN_POINT('',(9.,-5.,-6.12323399573677E-16));
#33149=CARTESIAN_POINT('',(8.855,-5.,-6.12323399573677E-16));
#33150=CARTESIAN_POINT('Origin',(9.,0.,0.));
#33151=CARTESIAN_POINT('Origin',(9.,0.,0.));
#33152=CARTESIAN_POINT('Origin',(3.9,0.,0.));
#33153=CARTESIAN_POINT('',(7.8,-8.2,-1.00421037530083E-15));
#33154=CARTESIAN_POINT('Origin',(7.8,0.,0.));
#33155=CARTESIAN_POINT('',(0.,-8.2,-1.00421037530083E-15));
#33156=CARTESIAN_POINT('',(3.9,-8.2,-1.00421037530083E-15));
#33157=CARTESIAN_POINT('Origin',(0.,0.,0.));
#33158=CARTESIAN_POINT('Origin',(0.,11.,0.));
#33159=CARTESIAN_POINT('',(5.55111512312578E-16,-11.,-1.34711147906209E-15));
#33160=CARTESIAN_POINT('Origin',(0.,0.,0.));
#33161=CARTESIAN_POINT('Origin',(3.8,0.,0.));
#33162=CARTESIAN_POINT('',(3.8,-11.,-1.34711147906209E-15));
#33163=CARTESIAN_POINT('Origin',(9.,0.,0.));
#33164=CARTESIAN_POINT('Origin',(7.8,8.2,0.));
#33165=CARTESIAN_POINT('',(0.,0.,0.));
#33166=CARTESIAN_POINT('Origin',(0.25,0.,0.));
#33167=CARTESIAN_POINT('',(0.5,-5.25,-6.42939569552361E-16));
#33168=CARTESIAN_POINT('Origin',(0.5,0.,0.));
#33169=CARTESIAN_POINT('',(0.,-5.25,-6.42939569552361E-16));
#33170=CARTESIAN_POINT('',(0.25,-5.25,-6.42939569552361E-16));
#33171=CARTESIAN_POINT('Origin',(0.,0.,0.));
#33172=CARTESIAN_POINT('Origin',(0.,12.,0.));
#33173=CARTESIAN_POINT('',(0.,-12.,-1.46957615897682E-15));
#33174=CARTESIAN_POINT('Origin',(0.,0.,0.));
#33175=CARTESIAN_POINT('Origin',(0.25,0.,0.));
#33176=CARTESIAN_POINT('',(0.5,-12.,-1.46957615897682E-15));
#33177=CARTESIAN_POINT('Origin',(0.5,0.,0.));
#33178=CARTESIAN_POINT('',(0.25,-12.,-1.46957615897682E-15));
#33179=CARTESIAN_POINT('Origin',(0.5,5.25,0.));
#33180=CARTESIAN_POINT('',(0.,0.,0.));
#33181=CARTESIAN_POINT('Origin',(1.5,0.,0.));
#33182=CARTESIAN_POINT('',(1.6,5.8,-7.10295143505465E-16));
#33183=CARTESIAN_POINT('Origin',(1.6,0.,0.));
#33184=CARTESIAN_POINT('',(1.4,6.,7.34788079488412E-16));
#33185=CARTESIAN_POINT('',(1.5,5.9,7.22541611496938E-16));
#33186=CARTESIAN_POINT('',(1.4,-6.,-7.34788079488412E-16));
#33187=CARTESIAN_POINT('Origin',(1.4,0.,0.));
#33188=CARTESIAN_POINT('Origin',(1.4,0.,0.));
#33189=CARTESIAN_POINT('Origin',(0.9,0.,0.));
#33190=CARTESIAN_POINT('',(0.2,-6.,-7.34788079488412E-16));
#33191=CARTESIAN_POINT('',(0.9,-6.,-7.34788079488412E-16));
#33192=CARTESIAN_POINT('Origin',(0.2,0.,0.));
#33193=CARTESIAN_POINT('Origin',(1.6,3.2,0.));
#33194=CARTESIAN_POINT('',(1.6,-3.2,-3.91886975727153E-16));
#33195=CARTESIAN_POINT('Origin',(1.6,0.,0.));
#33196=CARTESIAN_POINT('Origin',(0.8,0.,0.));
#33197=CARTESIAN_POINT('',(0.,-3.2,-3.91886975727153E-16));
#33198=CARTESIAN_POINT('',(0.8,-3.2,-3.91886975727153E-16));
#33199=CARTESIAN_POINT('Origin',(0.,0.,0.));
#33200=CARTESIAN_POINT('Origin',(0.,5.8,0.));
#33201=CARTESIAN_POINT('',(-1.21430643318376E-16,-5.8,-7.10295143505465E-16));
#33202=CARTESIAN_POINT('Origin',(0.,0.,0.));
#33203=CARTESIAN_POINT('Origin',(0.1,0.,0.));
#33204=CARTESIAN_POINT('',(0.1,-5.9,-7.22541611496938E-16));
#33205=CARTESIAN_POINT('',(0.,0.,0.));
#33206=CARTESIAN_POINT('Origin',(0.105,0.,0.));
#33207=CARTESIAN_POINT('',(0.,3.99234856522037E-16,3.26));
#33208=CARTESIAN_POINT('Origin',(0.,0.,0.));
#33209=CARTESIAN_POINT('',(0.21,-3.73517273739943E-16,3.05));
#33210=CARTESIAN_POINT('',(0.105,3.8637606513099E-16,3.155));
#33211=CARTESIAN_POINT('Origin',(0.21,0.,0.));
#33212=CARTESIAN_POINT('Origin',(0.,0.,0.));
#33213=CARTESIAN_POINT('',(4.99,3.73517273739943E-16,3.05));
#33214=CARTESIAN_POINT('',(0.,-3.73517273739943E-16,3.05));
#33215=CARTESIAN_POINT('Origin',(4.99,0.,0.));
#33216=CARTESIAN_POINT('Origin',(0.,0.,0.));
#33217=CARTESIAN_POINT('',(0.,-4.76709676493043,5.83800979439775E-16));
#33218=CARTESIAN_POINT('Origin',(0.,0.,0.));
#33219=CARTESIAN_POINT('Origin',(5.095,0.,0.));
#33220=CARTESIAN_POINT('',(5.2,-3.99234856522037E-16,3.26));
#33221=CARTESIAN_POINT('Origin',(5.2,0.,0.));
#33222=CARTESIAN_POINT('',(5.095,-3.8637606513099E-16,3.155));
#33223=CARTESIAN_POINT('Origin',(5.2,0.,0.));
#33224=CARTESIAN_POINT('',(5.2,-4.55709676493043,5.58083396657681E-16));
#33225=CARTESIAN_POINT('Origin',(5.2,0.,0.));
#33226=CARTESIAN_POINT('Origin',(5.14698723052002,0.,-1.51500018753453E-16));
#33227=CARTESIAN_POINT('',(5.12242284024924,-4.84634925793137,0.000544850078605702));
#33228=CARTESIAN_POINT('',(5.14698723052002,-4.75273145074145,-8.85041773342654E-16));
#33229=CARTESIAN_POINT('',(5.09683111434416,-4.81710063273169,-1.12843168478692));
#33230=CARTESIAN_POINT('Ctrl Pts',(5.12242284024924,-4.84634925793137,0.000544850078605714));
#33231=CARTESIAN_POINT('Ctrl Pts',(5.12258745506561,-4.84634360853001,-0.0466128059954816));
#33232=CARTESIAN_POINT('Ctrl Pts',(5.12261509827417,-4.84618263351447,-0.0937728862634767));
#33233=CARTESIAN_POINT('Ctrl Pts',(5.12249850969393,-4.84586645506482,-0.140950755812712));
#33234=CARTESIAN_POINT('Ctrl Pts',(5.1222390372062,-4.84516278744378,-0.245946966870691));
#33235=CARTESIAN_POINT('Ctrl Pts',(5.12126403884311,-4.84369122988508,-0.350884456461739));
#33236=CARTESIAN_POINT('Ctrl Pts',(5.1195137951287,-4.84146093806515,-0.455914997135786));
#33237=CARTESIAN_POINT('Ctrl Pts',(5.11919231896539,-4.84105128902516,-0.475206490639806));
#33238=CARTESIAN_POINT('Ctrl Pts',(5.11884478359864,-4.84061603078406,-0.494501019604373));
#33239=CARTESIAN_POINT('Ctrl Pts',(5.11847095209106,-4.84015520444964,-0.5137993676135));
#33240=CARTESIAN_POINT('Ctrl Pts',(5.11663697723163,-4.83789444286382,-0.60847486809847));
#33241=CARTESIAN_POINT('Ctrl Pts',(5.11417276747822,-4.83502173710584,-0.703081226948676));
#33242=CARTESIAN_POINT('Ctrl Pts',(5.11105950361714,-4.83155152799433,-0.797731355339415));
#33243=CARTESIAN_POINT('Ctrl Pts',(5.10808469285799,-4.82823564605754,-0.888172202262667));
#33244=CARTESIAN_POINT('Ctrl Pts',(5.10451721810229,-4.82437416311071,-0.978653212545341));
#33245=CARTESIAN_POINT('Ctrl Pts',(5.10036110005478,-4.81997832709177,-1.06922898060177));
#33246=CARTESIAN_POINT('Ctrl Pts',(5.09946985787141,-4.81903567954267,-1.08865214047379));
#33247=CARTESIAN_POINT('Ctrl Pts',(5.09855162625204,-4.81806845645995,-1.10807948523719));
#33248=CARTESIAN_POINT('Ctrl Pts',(5.097606577682,-4.81707676405073,-1.12751126351893));
#33249=CARTESIAN_POINT('',(5.09677740552866,-3.38580646785427,-3.60751378519044));
#33250=CARTESIAN_POINT('Origin',(5.09397446104004,0.,-3.03000037506907E-16));
#33251=CARTESIAN_POINT('',(5.09429707896,-1.43134944939545,-4.73604420895221));
#33252=CARTESIAN_POINT('Ctrl Pts',(5.09755445426771,-3.38498180226697,-3.60796213827666));
#33253=CARTESIAN_POINT('Ctrl Pts',(5.10208910805487,-3.306532374156,-3.65875518959754));
#33254=CARTESIAN_POINT('Ctrl Pts',(5.10600293671798,-3.22788838889819,-3.70900942659254));
#33255=CARTESIAN_POINT('Ctrl Pts',(5.10928749257359,-3.14899825590931,-3.75874007608228));
#33256=CARTESIAN_POINT('Ctrl Pts',(5.1125720484292,-3.07010812292044,-3.80847072557203));
#33257=CARTESIAN_POINT('Ctrl Pts',(5.1152275551448,-2.99097139609486,-3.8576781071415));
#33258=CARTESIAN_POINT('Ctrl Pts',(5.1172683027408,-2.91149242928002,-3.90640134624237));
#33259=CARTESIAN_POINT('Ctrl Pts',(5.1195258017243,-2.82357186176538,-3.96029956616864));
#33260=CARTESIAN_POINT('Ctrl Pts',(5.12102533344247,-2.73538901539391,-4.01351009532352));
#33261=CARTESIAN_POINT('Ctrl Pts',(5.12181201357767,-2.6468245785265,-4.06609184584734));
#33262=CARTESIAN_POINT('Ctrl Pts',(5.12201372622946,-2.62411577145884,-4.07957433238664));
#33263=CARTESIAN_POINT('Ctrl Pts',(5.12216874303548,-2.60138168140064,-4.09301556871597));
#33264=CARTESIAN_POINT('Ctrl Pts',(5.12227816274004,-2.57861993944308,-4.10641670396003));
#33265=CARTESIAN_POINT('Ctrl Pts',(5.12272295365878,-2.48609349589572,-4.1608922966428));
#33266=CARTESIAN_POINT('Ctrl Pts',(5.1224108220235,-2.39324441111108,-4.2146269541486));
#33267=CARTESIAN_POINT('Ctrl Pts',(5.12143116018516,-2.29992768622846,-4.26770105548192));
#33268=CARTESIAN_POINT('Ctrl Pts',(5.1207402031598,-2.23411125435542,-4.30513430208397));
#33269=CARTESIAN_POINT('Ctrl Pts',(5.11971882252206,-2.16812718645086,-4.34220177245049));
#33270=CARTESIAN_POINT('Ctrl Pts',(5.11840412361931,-2.10192539895917,-4.37893444709976));
#33271=CARTESIAN_POINT('Ctrl Pts',(5.11756105808869,-2.05947275449227,-4.40248968988531));
#33272=CARTESIAN_POINT('Ctrl Pts',(5.11659741488945,-2.01693068142318,-4.42590716144565));
#33273=CARTESIAN_POINT('Ctrl Pts',(5.1155040557362,-1.97428781828196,-4.44919441992967));
#33274=CARTESIAN_POINT('Ctrl Pts',(5.11337841852356,-1.89138435835654,-4.49446798174724));
#33275=CARTESIAN_POINT('Ctrl Pts',(5.11076604974616,-1.80824095512528,-4.53917184750963));
#33276=CARTESIAN_POINT('Ctrl Pts',(5.1076105966465,-1.72476531763046,-4.58337685908149));
#33277=CARTESIAN_POINT('Ctrl Pts',(5.10460439266534,-1.64523797691552,-4.62549102702422));
#33278=CARTESIAN_POINT('Ctrl Pts',(5.10110512412939,-1.5654088999758,-4.66715243744714));
#33279=CARTESIAN_POINT('Ctrl Pts',(5.09708531259065,-1.48523497413254,-4.7083994075618));
#33280=CARTESIAN_POINT('Ctrl Pts',(5.09618881912773,-1.46735468304869,-4.71759825649204));
#33281=CARTESIAN_POINT('Ctrl Pts',(5.09526652679194,-1.44945739634337,-4.72677639755234));
#33282=CARTESIAN_POINT('Ctrl Pts',(5.09431829354256,-1.43154291244923,-4.73593408953816));
#33283=CARTESIAN_POINT('',(5.09677740552865,1.43129534855037,-4.73595130605467));
#33284=CARTESIAN_POINT('Origin',(5.09397446104004,0.,-3.03000037506907E-16));
#33285=CARTESIAN_POINT('',(5.09429707895991,3.38585987370109,-3.60760708934543));
#33286=CARTESIAN_POINT('Ctrl Pts',(5.09755445426772,1.43209596650657,-4.73546130124953));
#33287=CARTESIAN_POINT('Ctrl Pts',(5.10208910805488,1.51530875334164,-4.69291862925353));
#33288=CARTESIAN_POINT('Ctrl Pts',(5.10600293671799,1.59815219185601,-4.64993805866292));
#33289=CARTESIAN_POINT('Ctrl Pts',(5.1092874925736,1.68066526415526,-4.60648252413149));
#33290=CARTESIAN_POINT('Ctrl Pts',(5.1125720484292,1.76317833645451,-4.56302698960007));
#33291=CARTESIAN_POINT('Ctrl Pts',(5.1152275551448,1.84536154236019,-4.5190962645815));
#33292=CARTESIAN_POINT('Ctrl Pts',(5.1172683027408,1.92729658858363,-4.47462707980373));
#33293=CARTESIAN_POINT('Ctrl Pts',(5.11952580172424,2.01793410001322,-4.42543474478548));
#33294=CARTESIAN_POINT('Ctrl Pts',(5.12102533344239,2.10810719319333,-4.37567142422865));
#33295=CARTESIAN_POINT('Ctrl Pts',(5.12181201357761,2.19792654335358,-4.325263247293));
#33296=CARTESIAN_POINT('Ctrl Pts',(5.12201372622942,2.22095712273921,-4.31233808675098));
#33297=CARTESIAN_POINT('Ctrl Pts',(5.12216874303546,2.24396461989036,-4.29937040539186));
#33298=CARTESIAN_POINT('Ctrl Pts',(5.12227816274004,2.26695121443263,-4.2863587262428));
#33299=CARTESIAN_POINT('Ctrl Pts',(5.12272295365878,2.36039168335589,-4.23346627195029));
#33300=CARTESIAN_POINT('Ctrl Pts',(5.1224108220235,2.45335180421185,-4.17992393456159));
#33301=CARTESIAN_POINT('Ctrl Pts',(5.12143116018516,2.5459736866908,-4.12564633088196));
#33302=CARTESIAN_POINT('Ctrl Pts',(5.12074020315979,2.61130004513081,-4.08736425219449));
#33303=CARTESIAN_POINT('Ctrl Pts',(5.11971882252206,2.6763934500745,-4.04875410832737));
#33304=CARTESIAN_POINT('Ctrl Pts',(5.11840412361931,2.74130577321557,-4.00978801590827));
#33305=CARTESIAN_POINT('Ctrl Pts',(5.1175610580887,2.78293153409362,-3.98480056873488));
#33306=CARTESIAN_POINT('Ctrl Pts',(5.11659741488945,2.82448269589182,-3.95966678850756));
#33307=CARTESIAN_POINT('Ctrl Pts',(5.1155040557362,2.8659714848941,-3.93438061497915));
#33308=CARTESIAN_POINT('Ctrl Pts',(5.11337841852354,2.94663126951159,-3.88522089353032));
#33309=CARTESIAN_POINT('Ctrl Pts',(5.1107660497461,3.02691765452577,-3.83556852705556));
#33310=CARTESIAN_POINT('Ctrl Pts',(5.10761059664638,3.10693813626994,-3.78537901017327));
#33311=CARTESIAN_POINT('Ctrl Pts',(5.10460439266523,3.18317374592452,-3.7375633967904));
#33312=CARTESIAN_POINT('Ctrl Pts',(5.1011051241293,3.25916812417756,-3.68926009341173));
#33313=CARTESIAN_POINT('Ctrl Pts',(5.09708531259058,3.33497601104708,-3.64045092196801));
#33314=CARTESIAN_POINT('Ctrl Pts',(5.09618881912768,3.35188259344778,-3.62956556012772));
#33315=CARTESIAN_POINT('Ctrl Pts',(5.09526652679191,3.36877974011778,-3.6186551257125));
#33316=CARTESIAN_POINT('Ctrl Pts',(5.09431829354256,3.3856677759642,-3.60771957355765));
#33317=CARTESIAN_POINT('',(5.09683109738054,4.81710063325383,-1.12843170492155));
#33318=CARTESIAN_POINT('Origin',(5.09397446104004,0.,-3.03000037506907E-16));
#33319=CARTESIAN_POINT('',(5.09435863143588,4.81720827487948,1.128405867392));
#33320=CARTESIAN_POINT('Ctrl Pts',(5.097606577682,4.81707676405073,-1.12751126351891));
#33321=CARTESIAN_POINT('Ctrl Pts',(5.10214583424673,4.82184006026792,-1.03417656102222));
#33322=CARTESIAN_POINT('Ctrl Pts',(5.10606427104759,4.82603945478669,-0.940942768451708));
#33323=CARTESIAN_POINT('Ctrl Pts',(5.10935323920574,4.82966233995838,-0.847757552481685));
#33324=CARTESIAN_POINT('Ctrl Pts',(5.11264220736389,4.83328522513008,-0.754572336511663));
#33325=CARTESIAN_POINT('Ctrl Pts',(5.11530193004546,4.83633165463593,-0.661435150975137));
#33326=CARTESIAN_POINT('Ctrl Pts',(5.11734647648754,4.83878768962393,-0.568243556567847));
#33327=CARTESIAN_POINT('Ctrl Pts',(5.11960814356782,4.84150454328205,-0.465155479480455));
#33328=CARTESIAN_POINT('Ctrl Pts',(5.12111134706416,4.84349472815332,-0.362183990119648));
#33329=CARTESIAN_POINT('Ctrl Pts',(5.12190089378603,4.84474960957374,-0.259196249019833));
#33330=CARTESIAN_POINT('Ctrl Pts',(5.12210335647361,4.84507139757935,-0.232787204091984));
#33331=CARTESIAN_POINT('Ctrl Pts',(5.12225906344213,4.84534481516978,-0.206376876932988));
#33332=CARTESIAN_POINT('Ctrl Pts',(5.12236910852286,4.84556967306519,-0.179962639911952));
#33333=CARTESIAN_POINT('Ctrl Pts',(5.12281641519127,4.84648366608875,-0.0725951475894643));
#33334=CARTESIAN_POINT('Ctrl Pts',(5.12250581136907,4.846594678656,0.0346815034442518));
#33335=CARTESIAN_POINT('Ctrl Pts',(5.12152637326862,4.84589982554879,0.142033144882093));
#33336=CARTESIAN_POINT('Ctrl Pts',(5.12083557404595,4.84540974456652,0.217748425331946));
#33337=CARTESIAN_POINT('Ctrl Pts',(5.1198137027769,4.8445190804778,0.293426134197082));
#33338=CARTESIAN_POINT('Ctrl Pts',(5.11849777244951,4.84322962374661,0.369125157802716));
#33339=CARTESIAN_POINT('Ctrl Pts',(5.11765391725392,4.8424027450438,0.417668012269155));
#33340=CARTESIAN_POINT('Ctrl Pts',(5.11668918025442,4.84141184227801,0.466219495085933));
#33341=CARTESIAN_POINT('Ctrl Pts',(5.1155944719316,4.84025777988173,0.514793214344727));
#33342=CARTESIAN_POINT('Ctrl Pts',(5.1134660840762,4.83801399280399,0.609232721205176));
#33343=CARTESIAN_POINT('Ctrl Pts',(5.11084994672088,4.83515680140141,0.703595379434204));
#33344=CARTESIAN_POINT('Ctrl Pts',(5.10769005829827,4.83170141167255,0.797996480817579));
#33345=CARTESIAN_POINT('Ctrl Pts',(5.10467957854565,4.82840940277069,0.887934024911113));
#33346=CARTESIAN_POINT('Ctrl Pts',(5.10117541306817,4.8245743529801,0.977906636196995));
#33347=CARTESIAN_POINT('Ctrl Pts',(5.09715037047566,4.82020789063866,1.06797075806217));
#33348=CARTESIAN_POINT('Ctrl Pts',(5.0962533412586,4.81923477191869,1.08804263230067));
#33349=CARTESIAN_POINT('Ctrl Pts',(5.0953305327574,4.81823525539394,1.10811886917062));
#33350=CARTESIAN_POINT('Ctrl Pts',(5.09438180624853,4.81720946415242,1.12819977138991));
#33351=CARTESIAN_POINT('',(5.09677740552871,3.38580646785444,3.60751378519034));
#33352=CARTESIAN_POINT('Origin',(5.09397446104004,0.,-3.03000037506907E-16));
#33353=CARTESIAN_POINT('',(5.09429707895988,1.43134944939528,4.73604420895232));
#33354=CARTESIAN_POINT('Ctrl Pts',(5.09755445426767,3.38498180226722,3.60796213827651));
#33355=CARTESIAN_POINT('Ctrl Pts',(5.10208910805484,3.3065323741562,3.65875518959743));
#33356=CARTESIAN_POINT('Ctrl Pts',(5.10600293671795,3.22788838889833,3.70900942659247));
#33357=CARTESIAN_POINT('Ctrl Pts',(5.10928749257356,3.14899825590938,3.75874007608226));
#33358=CARTESIAN_POINT('Ctrl Pts',(5.11257204842918,3.07010812292043,3.80847072557205));
#33359=CARTESIAN_POINT('Ctrl Pts',(5.11522755514478,2.99097139609477,3.85767810714158));
#33360=CARTESIAN_POINT('Ctrl Pts',(5.11726830274078,2.91149242927984,3.90640134624249));
#33361=CARTESIAN_POINT('Ctrl Pts',(5.11952580172432,2.82357186176373,3.96029956616967));
#33362=CARTESIAN_POINT('Ctrl Pts',(5.1210253334425,2.73538901539079,4.01351009532541));
#33363=CARTESIAN_POINT('Ctrl Pts',(5.12181201357769,2.64682457852191,4.06609184585008));
#33364=CARTESIAN_POINT('Ctrl Pts',(5.12201372622945,2.62411577145574,4.07957433238849));
#33365=CARTESIAN_POINT('Ctrl Pts',(5.12216874303546,2.60138168139903,4.09301556871694));
#33366=CARTESIAN_POINT('Ctrl Pts',(5.12227816274002,2.57861993944296,4.10641670396012));
#33367=CARTESIAN_POINT('Ctrl Pts',(5.12272295365876,2.48609349589551,4.16089229664294));
#33368=CARTESIAN_POINT('Ctrl Pts',(5.12241082202347,2.39324441111092,4.21462695414871));
#33369=CARTESIAN_POINT('Ctrl Pts',(5.12143116018513,2.29992768622834,4.26770105548201));
#33370=CARTESIAN_POINT('Ctrl Pts',(5.12074020315977,2.23411125435535,4.30513430208403));
#33371=CARTESIAN_POINT('Ctrl Pts',(5.11971882252203,2.16812718645086,4.34220177245051));
#33372=CARTESIAN_POINT('Ctrl Pts',(5.11840412361928,2.10192539895918,4.37893444709977));
#33373=CARTESIAN_POINT('Ctrl Pts',(5.11756105808867,2.05947275449225,4.40248968988534));
#33374=CARTESIAN_POINT('Ctrl Pts',(5.11659741488942,2.0169306814231,4.42590716144571));
#33375=CARTESIAN_POINT('Ctrl Pts',(5.11550405573616,1.97428781828179,4.44919441992978));
#33376=CARTESIAN_POINT('Ctrl Pts',(5.11337841852356,1.8913843583577,4.49446798174663));
#33377=CARTESIAN_POINT('Ctrl Pts',(5.11076604974621,1.80824095512778,4.53917184750831));
#33378=CARTESIAN_POINT('Ctrl Pts',(5.10761059664661,1.72476531763432,4.58337685907947));
#33379=CARTESIAN_POINT('Ctrl Pts',(5.10460439266551,1.64523797692054,4.62549102702161));
#33380=CARTESIAN_POINT('Ctrl Pts',(5.10110512412964,1.565408899982,4.66715243744393));
#33381=CARTESIAN_POINT('Ctrl Pts',(5.09708531259098,1.48523497413995,4.70839940755801));
#33382=CARTESIAN_POINT('Ctrl Pts',(5.09618881912794,1.46735468305352,4.71759825648959));
#33383=CARTESIAN_POINT('Ctrl Pts',(5.09526652679202,1.44945739634561,4.72677639755122));
#33384=CARTESIAN_POINT('Ctrl Pts',(5.09431829354251,1.43154291244888,4.73593408953836));
#33385=CARTESIAN_POINT('',(5.09677740552872,-1.43129534855014,4.73595130605479));
#33386=CARTESIAN_POINT('Origin',(5.09397446104004,0.,-3.03000037506907E-16));
#33387=CARTESIAN_POINT('',(5.09429707895997,-3.38585987370121,3.60760708934535));
#33388=CARTESIAN_POINT('Ctrl Pts',(5.09755445426766,-1.43209596650623,4.73546130124972));
#33389=CARTESIAN_POINT('Ctrl Pts',(5.10208910805483,-1.51530875334136,4.69291862925369));
#33390=CARTESIAN_POINT('Ctrl Pts',(5.10600293671795,-1.5981521918558,4.64993805866305));
#33391=CARTESIAN_POINT('Ctrl Pts',(5.10928749257356,-1.68066526415513,4.60648252413158));
#33392=CARTESIAN_POINT('Ctrl Pts',(5.11257204842917,-1.76317833645446,4.56302698960011));
#33393=CARTESIAN_POINT('Ctrl Pts',(5.11522755514477,-1.84536154236023,4.5190962645815));
#33394=CARTESIAN_POINT('Ctrl Pts',(5.11726830274077,-1.92729658858375,4.47462707980369));
#33395=CARTESIAN_POINT('Ctrl Pts',(5.11952580172431,-2.01793410001716,4.42543474478336));
#33396=CARTESIAN_POINT('Ctrl Pts',(5.12102533344249,-2.10810719320099,4.37567142422444));
#33397=CARTESIAN_POINT('Ctrl Pts',(5.12181201357768,-2.19792654336493,4.32526324728665));
#33398=CARTESIAN_POINT('Ctrl Pts',(5.12201372622944,-2.22095712274679,4.31233808674672));
#33399=CARTESIAN_POINT('Ctrl Pts',(5.12216874303545,-2.24396461989418,4.29937040538972));
#33400=CARTESIAN_POINT('Ctrl Pts',(5.12227816274001,-2.2669512144327,4.28635872624278));
#33401=CARTESIAN_POINT('Ctrl Pts',(5.12272295365876,-2.36039168335588,4.23346627195032));
#33402=CARTESIAN_POINT('Ctrl Pts',(5.12241082202347,-2.45335180421187,4.17992393456159));
#33403=CARTESIAN_POINT('Ctrl Pts',(5.12143116018513,-2.54597368669086,4.12564633088194));
#33404=CARTESIAN_POINT('Ctrl Pts',(5.12074020315977,-2.61130004513086,4.08736425219448));
#33405=CARTESIAN_POINT('Ctrl Pts',(5.11971882252203,-2.67639345007453,4.04875410832738));
#33406=CARTESIAN_POINT('Ctrl Pts',(5.11840412361928,-2.74130577321558,4.00978801590828));
#33407=CARTESIAN_POINT('Ctrl Pts',(5.11756105808867,-2.78293153409365,3.98480056873488));
#33408=CARTESIAN_POINT('Ctrl Pts',(5.11659741488943,-2.82448269589188,3.95966678850754));
#33409=CARTESIAN_POINT('Ctrl Pts',(5.11550405573617,-2.86597148489419,3.93438061497911));
#33410=CARTESIAN_POINT('Ctrl Pts',(5.11337841852351,-2.94663126951153,3.88522089353037));
#33411=CARTESIAN_POINT('Ctrl Pts',(5.11076604974608,-3.02691765452555,3.83556852705571));
#33412=CARTESIAN_POINT('Ctrl Pts',(5.10761059664637,-3.10693813626956,3.78537901017352));
#33413=CARTESIAN_POINT('Ctrl Pts',(5.10460439266523,-3.18317374592392,3.73756339679079));
#33414=CARTESIAN_POINT('Ctrl Pts',(5.10110512412932,-3.25916812417675,3.68926009341227));
#33415=CARTESIAN_POINT('Ctrl Pts',(5.09708531259061,-3.33497601104604,3.64045092196869));
#33416=CARTESIAN_POINT('Ctrl Pts',(5.09618881912769,-3.35188259344717,3.62956556012812));
#33417=CARTESIAN_POINT('Ctrl Pts',(5.0952665267919,-3.3687797401176,3.61865512571262));
#33418=CARTESIAN_POINT('Ctrl Pts',(5.09431829354252,-3.38566777596445,3.6077195735575));
#33419=CARTESIAN_POINT('',(5.09422149081015,-4.81720123716838,1.12962547313837));
#33420=CARTESIAN_POINT('Origin',(5.09397446104004,0.,-3.03000037506907E-16));
#33421=CARTESIAN_POINT('Ctrl Pts',(5.09438180624853,-4.81720946415242,1.12819977138992));
#33422=CARTESIAN_POINT('Ctrl Pts',(5.09878886055567,-4.82197450198674,1.03491933093676));
#33423=CARTESIAN_POINT('Ctrl Pts',(5.10263430365562,-4.82617320749278,0.941738192636836));
#33424=CARTESIAN_POINT('Ctrl Pts',(5.10594351391264,-4.82979238468145,0.848601343867398));
#33425=CARTESIAN_POINT('Ctrl Pts',(5.10925272416967,-4.83341156187012,0.75546449509796));
#33426=CARTESIAN_POINT('Ctrl Pts',(5.11202603583231,-4.8364512781726,0.662371388440315));
#33427=CARTESIAN_POINT('Ctrl Pts',(5.11431327464526,-4.83889682851293,0.569216691291326));
#33428=CARTESIAN_POINT('Ctrl Pts',(5.11595169894918,-4.84064865656489,0.502486921330922));
#33429=CARTESIAN_POINT('Ctrl Pts',(5.11733887369218,-4.84209375534294,0.435801442391284));
#33430=CARTESIAN_POINT('Ctrl Pts',(5.11849784929899,-4.84322957955454,0.369125161058667));
#33431=CARTESIAN_POINT('Ctrl Pts',(5.11958756105594,-4.84429752351292,0.306433653790524));
#33432=CARTESIAN_POINT('Ctrl Pts',(5.12047576221681,-4.84509205804993,0.243750068965635));
#33433=CARTESIAN_POINT('Ctrl Pts',(5.12114133368399,-4.8456119029517,0.181040444019433));
#33434=CARTESIAN_POINT('Ctrl Pts',(5.12178006274419,-4.8461107825791,0.120859889739829));
#33435=CARTESIAN_POINT('Ctrl Pts',(5.12221296107479,-4.84635639410279,0.0607049047250273));
#33436=CARTESIAN_POINT('Ctrl Pts',(5.12242284024924,-4.84634925793137,0.000544850078605714));
#33437=CARTESIAN_POINT('Ctrl Pts',(4.44772342888108,0.165392353541528,5.67801337205715));
#33438=CARTESIAN_POINT('Ctrl Pts',(4.69727026033307,0.931491616708207,5.2357057562419));
#33439=CARTESIAN_POINT('Ctrl Pts',(4.96928012765321,2.42096936008937,4.37575538014882));
#33440=CARTESIAN_POINT('Ctrl Pts',(4.78045253748373,3.81314196223624,3.57198415354091));
#33441=CARTESIAN_POINT('Ctrl Pts',(4.44772342888108,4.83460764645847,2.98224066578724));
#33442=CARTESIAN_POINT('Ctrl Pts',(4.5447241499808,0.110261569027686,5.63725117364547));
#33443=CARTESIAN_POINT('Ctrl Pts',(4.7983881862218,0.881878377310221,5.19312555764156));
#33444=CARTESIAN_POINT('Ctrl Pts',(5.07815075443906,2.389498397681,4.32537672517764));
#33445=CARTESIAN_POINT('Ctrl Pts',(4.8829428649688,3.79962864594736,3.50901750660556));
#33446=CARTESIAN_POINT('Ctrl Pts',(4.5447241499808,4.82687193937677,2.91411490666184));
#33447=CARTESIAN_POINT('Ctrl Pts',(4.64172487108053,0.0551307845138434,
5.59648897523378));
#33448=CARTESIAN_POINT('Ctrl Pts',(4.89950611211053,0.832265137912237,5.15054535904122));
#33449=CARTESIAN_POINT('Ctrl Pts',(5.18702138122492,2.35802743527264,4.27499807020645));
#33450=CARTESIAN_POINT('Ctrl Pts',(4.98543319245386,3.78611532965848,3.44605085967021));
#33451=CARTESIAN_POINT('Ctrl Pts',(4.64172487108053,4.81913623229508,2.84598914753644));
#33452=CARTESIAN_POINT('Ctrl Pts',(4.73872559218025,1.11022302462516E-15,
5.5557267768221));
#33453=CARTESIAN_POINT('Ctrl Pts',(5.00062403799926,0.782651898514251,5.10796516044089));
#33454=CARTESIAN_POINT('Ctrl Pts',(5.29589200801077,2.32655647286427,4.22461941523526));
#33455=CARTESIAN_POINT('Ctrl Pts',(5.08792351993893,3.7726020133696,3.38308421273486));
#33456=CARTESIAN_POINT('Ctrl Pts',(4.73872559218025,4.81140052521337,2.77786338841105));
#33457=CARTESIAN_POINT('',(4.73872559218025,4.81140052521337,2.77786338841105));
#33458=CARTESIAN_POINT('Ctrl Pts',(5.097554454267,3.38498180227162,3.60796213827396));
#33459=CARTESIAN_POINT('Ctrl Pts',(5.02981162260678,3.82780377487382,3.35078704750243));
#33460=CARTESIAN_POINT('Ctrl Pts',(4.91293516184791,4.29315964422862,3.0797989125881));
#33461=CARTESIAN_POINT('Ctrl Pts',(4.73872559218025,4.81140052521337,2.77786338841105));
#33462=CARTESIAN_POINT('',(4.45307482442111,4.81813466520579,2.99175134594783));
#33463=CARTESIAN_POINT('Ctrl Pts',(4.45307482442111,4.81813466520579,2.99175134594783));
#33464=CARTESIAN_POINT('Ctrl Pts',(4.50072369957731,4.81696840196052,2.95614749038523));
#33465=CARTESIAN_POINT('Ctrl Pts',(4.54835588589747,4.81582399363754,2.92051895860767));
#33466=CARTESIAN_POINT('Ctrl Pts',(4.64357232351903,4.81357928293661,2.84922335113861));
#33467=CARTESIAN_POINT('Ctrl Pts',(4.69115813327903,4.81247893359302,2.81355512622421));
#33468=CARTESIAN_POINT('Ctrl Pts',(4.73872559218025,4.81140052521337,2.77786338841105));
#33469=CARTESIAN_POINT('',(4.45307482442096,0.181865334794732,5.66850269189626));
#33470=CARTESIAN_POINT('Ctrl Pts',(4.45307670887188,4.81813292344043,2.99175235155653));
#33471=CARTESIAN_POINT('Ctrl Pts',(4.78160975160098,3.8045770857894,3.57692908726307));
#33472=CARTESIAN_POINT('Ctrl Pts',(4.96786706546316,2.42067099411741,4.37592764182305));
#33473=CARTESIAN_POINT('Ctrl Pts',(4.69893917059593,0.940653225099449,5.230416299171));
#33474=CARTESIAN_POINT('Ctrl Pts',(4.45307570990783,0.181866974811239,5.66850174503229));
#33475=CARTESIAN_POINT('',(4.73872559218025,1.5738093079395E-15,5.5557267768221));
#33476=CARTESIAN_POINT('Ctrl Pts',(4.73872559218025,2.80742846517038E-15,
5.5557267768221));
#33477=CARTESIAN_POINT('Ctrl Pts',(4.69115755784355,0.0303711148643061,
5.57450680196497));
#33478=CARTESIAN_POINT('Ctrl Pts',(4.64357117219491,0.060710895726737,5.59329407226952));
#33479=CARTESIAN_POINT('Ctrl Pts',(4.54835473372577,0.121332346083827,5.63088585282973));
#33480=CARTESIAN_POINT('Ctrl Pts',(4.50072312329429,0.151614988891,5.64969097803559));
#33481=CARTESIAN_POINT('Ctrl Pts',(4.45307482442137,0.181865334795011,5.6685026918961));
#33482=CARTESIAN_POINT('Ctrl Pts',(4.73872559218025,1.11022302462516E-15,
5.5557267768221));
#33483=CARTESIAN_POINT('Ctrl Pts',(4.91293516184791,0.520604274734674,5.2578847706982));
#33484=CARTESIAN_POINT('Ctrl Pts',(5.02725497143633,0.98767988560083,4.99065459457934));
#33485=CARTESIAN_POINT('Ctrl Pts',(5.09431829354185,1.43154291244451,4.73593408954086));
#33486=CARTESIAN_POINT('Ctrl Pts',(4.44772342888108,5.,2.69577270626991));
#33487=CARTESIAN_POINT('Ctrl Pts',(4.69727026033307,5.,1.8111574746394));
#33488=CARTESIAN_POINT('Ctrl Pts',(4.96948022596782,5.,0.0912172907134413));
#33489=CARTESIAN_POINT('Ctrl Pts',(4.78045253748373,5.,-1.51628573076257));
#33490=CARTESIAN_POINT('Ctrl Pts',(4.44772342888108,5.,-2.69577270626992));
#33491=CARTESIAN_POINT('Ctrl Pts',(4.5447241499808,4.93713350840446,2.72313626698363));
#33492=CARTESIAN_POINT('Ctrl Pts',(4.7983881862218,4.93831784661493,1.83283370102193));
#33493=CARTESIAN_POINT('Ctrl Pts',(5.07834742005573,4.94063410426251,0.0932810725788978));
#33494=CARTESIAN_POINT('Ctrl Pts',(4.8829428649688,4.93871262601842,-1.5360661790347));
#33495=CARTESIAN_POINT('Ctrl Pts',(4.5447241499808,4.93713350840446,-2.72313626698363));
#33496=CARTESIAN_POINT('Ctrl Pts',(4.64172487108053,4.87426701680892,2.75049982769734));
#33497=CARTESIAN_POINT('Ctrl Pts',(4.89950611211053,4.87663569322986,1.85450992740445));
#33498=CARTESIAN_POINT('Ctrl Pts',(5.18721461414363,4.88126820852503,0.0953448544443543));
#33499=CARTESIAN_POINT('Ctrl Pts',(4.98543319245386,4.87742525203684,-1.55584662730683));
#33500=CARTESIAN_POINT('Ctrl Pts',(4.64172487108053,4.87426701680891,-2.75049982769734));
#33501=CARTESIAN_POINT('Ctrl Pts',(4.73872559218025,4.81140052521337,2.77786338841105));
#33502=CARTESIAN_POINT('Ctrl Pts',(5.00062403799926,4.81495353984479,1.87618615378698));
#33503=CARTESIAN_POINT('Ctrl Pts',(5.29608180823153,4.82190231278754,0.0974086363098105));
#33504=CARTESIAN_POINT('Ctrl Pts',(5.08792351993893,4.81613787805526,-1.57562707557896));
#33505=CARTESIAN_POINT('Ctrl Pts',(4.73872559218025,4.81140052521337,-2.77786338841105));
#33506=CARTESIAN_POINT('',(4.73872559218025,4.81140052521337,-2.77786338841105));
#33507=CARTESIAN_POINT('Ctrl Pts',(5.0976065776813,4.81707676405072,-1.12751126352421));
#33508=CARTESIAN_POINT('Ctrl Pts',(5.02983861611708,4.8157680729232,-1.63958805258426));
#33509=CARTESIAN_POINT('Ctrl Pts',(4.91293516184791,4.81376391896329,-2.1780858581101));
#33510=CARTESIAN_POINT('Ctrl Pts',(4.73872559218025,4.81140052521337,-2.77786338841105));
#33511=CARTESIAN_POINT('',(4.45307482442111,5.,-2.67675134594873));
#33512=CARTESIAN_POINT('Ctrl Pts',(4.45307482442111,5.,-2.67675134594873));
#33513=CARTESIAN_POINT('Ctrl Pts',(4.50072369957984,4.96858302498581,-2.69354326013303));
#33514=CARTESIAN_POINT('Ctrl Pts',(4.54835588589865,4.9371556072063,-2.71036643934133));
#33515=CARTESIAN_POINT('Ctrl Pts',(4.64357232350986,4.87428944461622,-2.74407026658104));
#33516=CARTESIAN_POINT('Ctrl Pts',(4.69115813327444,4.84284968105765,-2.76095144855526));
#33517=CARTESIAN_POINT('Ctrl Pts',(4.73872559218026,4.81140052521337,-2.77786338841105));
#33518=CARTESIAN_POINT('',(4.45307482442096,5.,2.67675134594813));
#33519=CARTESIAN_POINT('Ctrl Pts',(4.45307671877181,5.,-2.67674933668223));
#33520=CARTESIAN_POINT('Ctrl Pts',(4.78161097872069,5.,-1.50639610513671));
#33521=CARTESIAN_POINT('Ctrl Pts',(4.96806593665806,5.,0.0915620558803535));
#33522=CARTESIAN_POINT('Ctrl Pts',(4.69894039771564,5.,1.80057831867916));
#33523=CARTESIAN_POINT('Ctrl Pts',(4.45307572309982,5.,2.67674944962055));
#33524=CARTESIAN_POINT('Ctrl Pts',(4.73872559218025,4.81140052521337,2.77786338841105));
#33525=CARTESIAN_POINT('Ctrl Pts',(4.69115755784416,4.84285006150256,2.76095124396896));
#33526=CARTESIAN_POINT('Ctrl Pts',(4.64357117219626,4.8742902052848,2.74406985814937));
#33527=CARTESIAN_POINT('Ctrl Pts',(4.54835473372633,4.93715636740249,2.7103660324057));
#33528=CARTESIAN_POINT('Ctrl Pts',(4.50072312329534,4.96858340495538,2.69354305704407));
#33529=CARTESIAN_POINT('Ctrl Pts',(4.45307482442137,5.,2.67675134594781));
#33530=CARTESIAN_POINT('Ctrl Pts',(4.73872559218025,4.81140052521337,2.77786338841105));
#33531=CARTESIAN_POINT('Ctrl Pts',(4.91293516184791,4.81376391896329,2.1780858581101));
#33532=CARTESIAN_POINT('Ctrl Pts',(5.02729096278339,4.81587290945609,1.63996307009543));
#33533=CARTESIAN_POINT('Ctrl Pts',(5.09438180624785,4.81720946415241,1.12819977139512));
#33534=CARTESIAN_POINT('Origin',(4.82293768228025,0.,0.));
#33535=CARTESIAN_POINT('Origin',(4.82293768228025,0.,0.));
#33536=CARTESIAN_POINT('Ctrl Pts',(4.73872559218025,4.81140052521337,-2.77786338841105));
#33537=CARTESIAN_POINT('Ctrl Pts',(4.91293516184791,4.29315964422862,-3.0797989125881));
#33538=CARTESIAN_POINT('Ctrl Pts',(5.02725497143633,3.82819371761882,-3.3506831690269));
#33539=CARTESIAN_POINT('Ctrl Pts',(5.09431829354185,3.38566777596886,-3.60771957355494));
#33540=CARTESIAN_POINT('Origin',(4.82293768228025,0.,0.));
#33541=CARTESIAN_POINT('',(4.73872559218025,-8.93429006522259E-16,-5.5557267768221));
#33542=CARTESIAN_POINT('Ctrl Pts',(4.73872559218025,2.80742846517038E-15,
-5.5557267768221));
#33543=CARTESIAN_POINT('Ctrl Pts',(4.91293516184791,-0.520604274734672,
-5.2578847706982));
#33544=CARTESIAN_POINT('Ctrl Pts',(5.02725497143632,-0.98767988560083,-4.99065459457934));
#33545=CARTESIAN_POINT('Ctrl Pts',(5.09431829354185,-1.43154291244451,-4.73593408954086));
#33546=CARTESIAN_POINT('Ctrl Pts',(5.097554454267,1.43209596650185,-4.73546130125224));
#33547=CARTESIAN_POINT('Ctrl Pts',(5.02981162260678,0.987964818372043,-4.99036883349392));
#33548=CARTESIAN_POINT('Ctrl Pts',(4.91293516184791,0.52060427473467,-5.2578847706982));
#33549=CARTESIAN_POINT('Ctrl Pts',(4.73872559218025,-3.19189119579733E-15,
-5.5557267768221));
#33550=CARTESIAN_POINT('Origin',(4.82293768228025,0.,0.));
#33551=CARTESIAN_POINT('',(4.73872559218025,-4.81140052521337,-2.77786338841105));
#33552=CARTESIAN_POINT('Ctrl Pts',(4.73872559218025,-4.81140052521337,-2.77786338841105));
#33553=CARTESIAN_POINT('Ctrl Pts',(4.91293516184791,-4.81376391896329,-2.1780858581101));
#33554=CARTESIAN_POINT('Ctrl Pts',(5.02983861611708,-4.8157680729232,-1.63958805258425));
#33555=CARTESIAN_POINT('Ctrl Pts',(5.0976065776813,-4.81707676405072,-1.12751126352421));
#33556=CARTESIAN_POINT('Ctrl Pts',(5.097554454267,-3.38498180227163,-3.60796213827395));
#33557=CARTESIAN_POINT('Ctrl Pts',(5.02981162260678,-3.82780377487383,-3.35078704750243));
#33558=CARTESIAN_POINT('Ctrl Pts',(4.91293516184791,-4.29315964422862,-3.0797989125881));
#33559=CARTESIAN_POINT('Ctrl Pts',(4.73872559218025,-4.81140052521337,-2.77786338841105));
#33560=CARTESIAN_POINT('Origin',(4.82293768228025,0.,0.));
#33561=CARTESIAN_POINT('',(4.73872559218025,-4.81140052521338,2.77786338841105));
#33562=CARTESIAN_POINT('Ctrl Pts',(4.73872559218025,-4.81140052521338,2.77786338841104));
#33563=CARTESIAN_POINT('Ctrl Pts',(4.91293516184791,-4.29315964422862,3.0797989125881));
#33564=CARTESIAN_POINT('Ctrl Pts',(5.02725497143633,-3.82819371761882,3.3506831690269));
#33565=CARTESIAN_POINT('Ctrl Pts',(5.09431829354185,-3.38566777596886,3.60771957355494));
#33566=CARTESIAN_POINT('Ctrl Pts',(5.09438180624785,-4.81720946415241,1.12819977139512));
#33567=CARTESIAN_POINT('Ctrl Pts',(5.02729096278339,-4.81587290945609,1.63996307009543));
#33568=CARTESIAN_POINT('Ctrl Pts',(4.91293516184791,-4.81376391896329,2.1780858581101));
#33569=CARTESIAN_POINT('Ctrl Pts',(4.73872559218025,-4.81140052521337,2.77786338841105));
#33570=CARTESIAN_POINT('Origin',(4.82293768228025,0.,0.));
#33571=CARTESIAN_POINT('Ctrl Pts',(5.097554454267,-1.43209596650185,4.73546130125224));
#33572=CARTESIAN_POINT('Ctrl Pts',(5.02981162260678,-0.987964818372044,
4.99036883349392));
#33573=CARTESIAN_POINT('Ctrl Pts',(4.91293516184791,-0.520604274734671,
5.2578847706982));
#33574=CARTESIAN_POINT('Ctrl Pts',(4.73872559218025,1.94289029309402E-15,
5.5557267768221));
#33575=CARTESIAN_POINT('Ctrl Pts',(4.44772342888108,4.83460764645847,-2.98224066578724));
#33576=CARTESIAN_POINT('Ctrl Pts',(4.69727026033307,4.06850838329179,-3.4245482816025));
#33577=CARTESIAN_POINT('Ctrl Pts',(4.96928012765321,2.57903063991063,-4.28449865769557));
#33578=CARTESIAN_POINT('Ctrl Pts',(4.78045253748373,1.18685803776376,-5.08826988430348));
#33579=CARTESIAN_POINT('Ctrl Pts',(4.44772342888108,0.165392353541524,-5.67801337205715));
#33580=CARTESIAN_POINT('Ctrl Pts',(4.5447241499808,4.82687193937677,-2.91411490666184));
#33581=CARTESIAN_POINT('Ctrl Pts',(4.7983881862218,4.05643946930471,-3.36029185661963));
#33582=CARTESIAN_POINT('Ctrl Pts',(5.07815075443906,2.55113692610127,-4.23205467728278));
#33583=CARTESIAN_POINT('Ctrl Pts',(4.8829428649688,1.13908398007106,-5.04508368564026));
#33584=CARTESIAN_POINT('Ctrl Pts',(4.5447241499808,0.110261569027681,-5.63725117364547));
#33585=CARTESIAN_POINT('Ctrl Pts',(4.64172487108053,4.81913623229507,-2.84598914753645));
#33586=CARTESIAN_POINT('Ctrl Pts',(4.89950611211053,4.04437055531762,-3.29603543163677));
#33587=CARTESIAN_POINT('Ctrl Pts',(5.18702138122492,2.52324321229191,-4.17961069687));
#33588=CARTESIAN_POINT('Ctrl Pts',(4.98543319245386,1.09130992237836,-5.00189748697704));
#33589=CARTESIAN_POINT('Ctrl Pts',(4.64172487108053,0.0551307845138391,
-5.59648897523378));
#33590=CARTESIAN_POINT('Ctrl Pts',(4.73872559218025,4.81140052521337,-2.77786338841105));
#33591=CARTESIAN_POINT('Ctrl Pts',(5.00062403799926,4.03230164133054,-3.23177900665391));
#33592=CARTESIAN_POINT('Ctrl Pts',(5.29589200801077,2.49534949848256,-4.12716671645721));
#33593=CARTESIAN_POINT('Ctrl Pts',(5.08792351993893,1.04353586468566,-4.95871128831382));
#33594=CARTESIAN_POINT('Ctrl Pts',(4.73872559218025,-3.19189119579733E-15,
-5.5557267768221));
#33595=CARTESIAN_POINT('',(4.45307482442111,0.181865334794207,-5.66850269189656));
#33596=CARTESIAN_POINT('Ctrl Pts',(4.45307482442111,0.181865334794213,-5.66850269189656));
#33597=CARTESIAN_POINT('Ctrl Pts',(4.50072369959053,0.151614623018565,-5.64969075051213));
#33598=CARTESIAN_POINT('Ctrl Pts',(4.54835588590384,0.121331613565481,-5.63088539794606));
#33599=CARTESIAN_POINT('Ctrl Pts',(4.64357232350899,0.0607101616799395,
-5.59329361772685));
#33600=CARTESIAN_POINT('Ctrl Pts',(4.69115813327399,0.0303707474648052,
-5.57450657478309));
#33601=CARTESIAN_POINT('Ctrl Pts',(4.73872559218025,-8.93429006522259E-16,
-5.5557267768221));
#33602=CARTESIAN_POINT('',(4.45307482442096,4.81813466520527,-2.99175134594813));
#33603=CARTESIAN_POINT('Ctrl Pts',(4.45307670887187,0.18186707655957,-5.66850168628786));
#33604=CARTESIAN_POINT('Ctrl Pts',(4.78160975160098,1.1954229142106,-5.08332495058132));
#33605=CARTESIAN_POINT('Ctrl Pts',(4.96786706546316,2.57932900588259,-4.28432639602134));
#33606=CARTESIAN_POINT('Ctrl Pts',(4.69893917059593,4.05934677490055,-3.42983773867339));
#33607=CARTESIAN_POINT('Ctrl Pts',(4.45307570990783,4.81813302518876,-2.9917522928121));
#33608=CARTESIAN_POINT('Ctrl Pts',(4.73872559218025,4.81140052521337,-2.77786338841105));
#33609=CARTESIAN_POINT('Ctrl Pts',(4.69115755784131,4.81247894663871,-2.81355555799791));
#33610=CARTESIAN_POINT('Ctrl Pts',(4.64357117219035,4.81357930955906,-2.84922421412404));
#33611=CARTESIAN_POINT('Ctrl Pts',(4.54835473372485,4.81582402131905,-2.92051982042491));
#33612=CARTESIAN_POINT('Ctrl Pts',(4.5007231232927,4.81696841606511,-2.95614792099309));
#33613=CARTESIAN_POINT('Ctrl Pts',(4.45307482442137,4.81813466520499,-2.99175134594829));
#33614=CARTESIAN_POINT('Origin',(4.45307482442111,5.,-2.67675134594873));
#33615=CARTESIAN_POINT('',(4.45307482442096,5.,-2.67675134594813));
#33616=CARTESIAN_POINT('Origin',(4.73872559218025,-8.93429006522259E-16,
-5.5557267768221));
#33617=CARTESIAN_POINT('',(4.45307482442096,-0.181865334794733,-5.66850269189626));
#33618=CARTESIAN_POINT('Ctrl Pts',(4.73872559218025,2.80742846517038E-15,
-5.5557267768221));
#33619=CARTESIAN_POINT('Ctrl Pts',(4.69115755784503,-0.0303711148633555,
-5.57450680196439));
#33620=CARTESIAN_POINT('Ctrl Pts',(4.64357117219794,-0.0607108957248108,
-5.59329407226833));
#33621=CARTESIAN_POINT('Ctrl Pts',(4.54835473372581,-0.121332346083798,
-5.63088585282971));
#33622=CARTESIAN_POINT('Ctrl Pts',(4.50072312329487,-0.151614988890633,
-5.64969097803537));
#33623=CARTESIAN_POINT('Ctrl Pts',(4.45307482442137,-0.181865334795012,
-5.6685026918961));
#33624=CARTESIAN_POINT('',(4.45307482442096,0.18186533479473,-5.66850269189626));
#33625=CARTESIAN_POINT('Origin',(4.45307482442111,4.81813466520579,2.99175134594783));
#33626=CARTESIAN_POINT('',(4.45307482442096,4.81813466520527,2.99175134594813));
#33627=CARTESIAN_POINT('Origin',(4.73872559218025,-4.81140052521337,-2.77786338841105));
#33628=CARTESIAN_POINT('',(4.45307482442111,-4.81813466520579,-2.99175134594783));
#33629=CARTESIAN_POINT('Ctrl Pts',(4.45307482442111,-4.81813466520579,-2.99175134594783));
#33630=CARTESIAN_POINT('Ctrl Pts',(4.50072369957741,-4.81696840196052,-2.95614749038515));
#33631=CARTESIAN_POINT('Ctrl Pts',(4.54835588589733,-4.81582399363755,-2.92051895860778));
#33632=CARTESIAN_POINT('Ctrl Pts',(4.64357232351839,-4.81357928293662,-2.84922335113908));
#33633=CARTESIAN_POINT('Ctrl Pts',(4.69115813327887,-4.81247893359302,-2.81355512622433));
#33634=CARTESIAN_POINT('Ctrl Pts',(4.73872559218025,-4.81140052521337,-2.77786338841105));
#33635=CARTESIAN_POINT('',(4.45307482442096,-5.,-2.67675134594813));
#33636=CARTESIAN_POINT('Ctrl Pts',(4.73872559218026,-4.81140052521337,-2.77786338841105));
#33637=CARTESIAN_POINT('Ctrl Pts',(4.69115755784151,-4.84285006150431,-2.76095124396802));
#33638=CARTESIAN_POINT('Ctrl Pts',(4.64357117219061,-4.87429020528853,-2.74406985814738));
#33639=CARTESIAN_POINT('Ctrl Pts',(4.54835473372593,-4.93715636740275,-2.71036603240556));
#33640=CARTESIAN_POINT('Ctrl Pts',(4.5007231232952,-4.96858340495548,-2.69354305704402));
#33641=CARTESIAN_POINT('Ctrl Pts',(4.45307482442137,-5.,-2.67675134594781));
#33642=CARTESIAN_POINT('',(4.45307482442096,-4.81813466520527,-2.99175134594813));
#33643=CARTESIAN_POINT('Origin',(4.45307482442111,-0.181865334794209,5.66850269189656));
#33644=CARTESIAN_POINT('',(4.45307482442111,-0.181865334794209,5.66850269189656));
#33645=CARTESIAN_POINT('',(4.45307482442096,-0.181865334794732,5.66850269189626));
#33646=CARTESIAN_POINT('Ctrl Pts',(4.45307482442111,-0.181865334794216,
5.66850269189656));
#33647=CARTESIAN_POINT('Ctrl Pts',(4.50072369958569,-0.151614623021643,
5.64969075051405));
#33648=CARTESIAN_POINT('Ctrl Pts',(4.54835588590163,-0.121331613566889,
5.63088539794693));
#33649=CARTESIAN_POINT('Ctrl Pts',(4.64357232351274,-0.0607101616775566,
5.59329361772537));
#33650=CARTESIAN_POINT('Ctrl Pts',(4.69115813327592,-0.0303707474635743,
5.57450657478233));
#33651=CARTESIAN_POINT('Ctrl Pts',(4.73872559218025,-2.12704816375314E-15,
5.5557267768221));
#33652=CARTESIAN_POINT('Origin',(4.73872559218025,-4.81140052521338,2.77786338841105));
#33653=CARTESIAN_POINT('',(4.45307482442111,-5.,2.67675134594873));
#33654=CARTESIAN_POINT('Ctrl Pts',(4.45307482442111,-5.,2.67675134594873));
#33655=CARTESIAN_POINT('Ctrl Pts',(4.50072369957508,-4.96858302498895,2.69354326013135));
#33656=CARTESIAN_POINT('Ctrl Pts',(4.54835588589647,-4.93715560720775,2.71036643934055));
#33657=CARTESIAN_POINT('Ctrl Pts',(4.64357232351721,-4.87428944461137,2.74407026658364));
#33658=CARTESIAN_POINT('Ctrl Pts',(4.6911581332779,-4.84284968105536,2.76095144855649));
#33659=CARTESIAN_POINT('Ctrl Pts',(4.73872559218025,-4.81140052521337,2.77786338841105));
#33660=CARTESIAN_POINT('',(4.45307482442096,-4.81813466520527,2.99175134594813));
#33661=CARTESIAN_POINT('Ctrl Pts',(4.73872559218025,-4.81140052521338,2.77786338841104));
#33662=CARTESIAN_POINT('Ctrl Pts',(4.69115755784599,-4.81247894663861,2.81355555799439));
#33663=CARTESIAN_POINT('Ctrl Pts',(4.64357117219958,-4.81357930955884,2.84922421411712));
#33664=CARTESIAN_POINT('Ctrl Pts',(4.54835473372284,-4.8158240213191,2.92051982042641));
#33665=CARTESIAN_POINT('Ctrl Pts',(4.50072312328868,-4.81696841606522,2.95614792099609));
#33666=CARTESIAN_POINT('Ctrl Pts',(4.45307482442137,-4.81813466520499,2.99175134594829));
#33667=CARTESIAN_POINT('',(4.45307482442096,-5.,2.67675134594813));
#33668=CARTESIAN_POINT('Ctrl Pts',(4.44772342888108,-4.83460764645848,2.98224066578723));
#33669=CARTESIAN_POINT('Ctrl Pts',(4.69727026033307,-4.0685083832918,3.42454828160249));
#33670=CARTESIAN_POINT('Ctrl Pts',(4.96928012765321,-2.57903063991063,4.28449865769556));
#33671=CARTESIAN_POINT('Ctrl Pts',(4.78045253748373,-1.18685803776377,5.08826988430348));
#33672=CARTESIAN_POINT('Ctrl Pts',(4.44772342888108,-0.165392353541525,
5.67801337205715));
#33673=CARTESIAN_POINT('Ctrl Pts',(4.5447241499808,-4.82687193937678,2.91411490666184));
#33674=CARTESIAN_POINT('Ctrl Pts',(4.7983881862218,-4.05643946930472,3.36029185661963));
#33675=CARTESIAN_POINT('Ctrl Pts',(5.07815075443907,-2.55113692610128,4.23205467728278));
#33676=CARTESIAN_POINT('Ctrl Pts',(4.8829428649688,-1.13908398007107,5.04508368564026));
#33677=CARTESIAN_POINT('Ctrl Pts',(4.5447241499808,-0.110261569027683,5.63725117364547));
#33678=CARTESIAN_POINT('Ctrl Pts',(4.64172487108053,-4.81913623229508,2.84598914753644));
#33679=CARTESIAN_POINT('Ctrl Pts',(4.89950611211053,-4.04437055531763,3.29603543163677));
#33680=CARTESIAN_POINT('Ctrl Pts',(5.18702138122492,-2.52324321229192,4.17961069686999));
#33681=CARTESIAN_POINT('Ctrl Pts',(4.98543319245386,-1.09130992237837,5.00189748697704));
#33682=CARTESIAN_POINT('Ctrl Pts',(4.64172487108053,-0.0551307845138405,
5.59648897523378));
#33683=CARTESIAN_POINT('Ctrl Pts',(4.73872559218025,-4.81140052521338,2.77786338841104));
#33684=CARTESIAN_POINT('Ctrl Pts',(5.00062403799926,-4.03230164133055,3.2317790066539));
#33685=CARTESIAN_POINT('Ctrl Pts',(5.29589200801077,-2.49534949848256,4.12716671645721));
#33686=CARTESIAN_POINT('Ctrl Pts',(5.08792351993893,-1.04353586468567,4.95871128831382));
#33687=CARTESIAN_POINT('Ctrl Pts',(4.73872559218025,1.94289029309402E-15,
5.5557267768221));
#33688=CARTESIAN_POINT('Ctrl Pts',(4.45307670887187,-0.181867076559572,
5.66850168628786));
#33689=CARTESIAN_POINT('Ctrl Pts',(4.78160975160098,-1.1954229142106,5.08332495058132));
#33690=CARTESIAN_POINT('Ctrl Pts',(4.96786706546316,-2.57932900588259,4.28432639602133));
#33691=CARTESIAN_POINT('Ctrl Pts',(4.69893917059593,-4.05934677490055,3.42983773867339));
#33692=CARTESIAN_POINT('Ctrl Pts',(4.45307570990783,-4.81813302518876,2.9917522928121));
#33693=CARTESIAN_POINT('Origin',(0.,-4.90906733260264,2.83425134594813));
#33694=CARTESIAN_POINT('',(0.528943702130891,-4.81813466520527,2.99175134594813));
#33695=CARTESIAN_POINT('',(0.528943702130891,-5.,2.67675134594813));
#33696=CARTESIAN_POINT('Ctrl Pts',(0.528943702130891,-4.81813466520527,
2.99175134594813));
#33697=CARTESIAN_POINT('Ctrl Pts',(0.525532604501329,-4.90906733260263,
2.83425134594813));
#33698=CARTESIAN_POINT('Ctrl Pts',(0.528943702130891,-5.,2.67675134594813));
#33699=CARTESIAN_POINT('',(0.,-5.,2.67675134594813));
#33700=CARTESIAN_POINT('',(0.,-4.81813466520527,2.99175134594813));
#33701=CARTESIAN_POINT('Ctrl Pts',(4.44772342888108,-5.,-2.69577270626992));
#33702=CARTESIAN_POINT('Ctrl Pts',(4.78045253748373,-5.,-1.51628573076256));
#33703=CARTESIAN_POINT('Ctrl Pts',(4.96948022596782,-5.,0.0912172907134438));
#33704=CARTESIAN_POINT('Ctrl Pts',(4.69727026033307,-5.,1.8111574746394));
#33705=CARTESIAN_POINT('Ctrl Pts',(4.44772342888108,-5.,2.69577270626992));
#33706=CARTESIAN_POINT('Ctrl Pts',(4.5447241499808,-4.93713350840446,-2.72313626698363));
#33707=CARTESIAN_POINT('Ctrl Pts',(4.8829428649688,-4.93871262601842,-1.53606617903469));
#33708=CARTESIAN_POINT('Ctrl Pts',(5.07834742005573,-4.94063410426251,0.0932810725788998));
#33709=CARTESIAN_POINT('Ctrl Pts',(4.7983881862218,-4.93831784661493,1.83283370102193));
#33710=CARTESIAN_POINT('Ctrl Pts',(4.5447241499808,-4.93713350840446,2.72313626698363));
#33711=CARTESIAN_POINT('Ctrl Pts',(4.64172487108053,-4.87426701680892,-2.75049982769734));
#33712=CARTESIAN_POINT('Ctrl Pts',(4.98543319245387,-4.87742525203684,-1.55584662730683));
#33713=CARTESIAN_POINT('Ctrl Pts',(5.18721461414363,-4.88126820852503,0.0953448544443579));
#33714=CARTESIAN_POINT('Ctrl Pts',(4.89950611211053,-4.87663569322986,1.85450992740445));
#33715=CARTESIAN_POINT('Ctrl Pts',(4.64172487108053,-4.87426701680892,2.75049982769734));
#33716=CARTESIAN_POINT('Ctrl Pts',(4.73872559218025,-4.81140052521337,-2.77786338841105));
#33717=CARTESIAN_POINT('Ctrl Pts',(5.08792351993893,-4.81613787805526,-1.57562707557896));
#33718=CARTESIAN_POINT('Ctrl Pts',(5.29608180823153,-4.82190231278754,0.0974086363098129));
#33719=CARTESIAN_POINT('Ctrl Pts',(5.00062403799926,-4.81495353984479,1.87618615378698));
#33720=CARTESIAN_POINT('Ctrl Pts',(4.73872559218025,-4.81140052521337,2.77786338841105));
#33721=CARTESIAN_POINT('Ctrl Pts',(4.45307572309967,-5.,2.67674944962107));
#33722=CARTESIAN_POINT('Ctrl Pts',(4.6989403977156,-5.,1.80057831867945));
#33723=CARTESIAN_POINT('Ctrl Pts',(4.96806593665806,-5.,0.091562055880635));
#33724=CARTESIAN_POINT('Ctrl Pts',(4.78161097872072,-5.,-1.50639610513643));
#33725=CARTESIAN_POINT('Ctrl Pts',(4.45307671877196,-5.,-2.67674933668171));
#33726=CARTESIAN_POINT('Origin',(0.,-1.56125112837913E-16,5.66850269189626));
#33727=CARTESIAN_POINT('',(0.528943702130891,0.181865334794732,5.66850269189626));
#33728=CARTESIAN_POINT('',(0.528943702130891,-0.181865334794732,5.66850269189626));
#33729=CARTESIAN_POINT('Ctrl Pts',(0.528943702130891,0.181865334794732,
5.66850269189626));
#33730=CARTESIAN_POINT('Ctrl Pts',(0.525532604501329,-1.14491749414469E-15,
5.66850269189626));
#33731=CARTESIAN_POINT('Ctrl Pts',(0.528943702130891,-0.181865334794732,
5.66850269189626));
#33732=CARTESIAN_POINT('',(0.,-0.181865334794732,5.66850269189626));
#33733=CARTESIAN_POINT('',(0.,0.181865334794732,5.66850269189626));
#33734=CARTESIAN_POINT('Origin',(0.,-4.90906733260263,-2.83425134594813));
#33735=CARTESIAN_POINT('',(0.52894370213089,-5.,-2.67675134594813));
#33736=CARTESIAN_POINT('',(0.528943702130891,-4.81813466520527,-2.99175134594813));
#33737=CARTESIAN_POINT('Ctrl Pts',(0.52894370213089,-5.,-2.67675134594813));
#33738=CARTESIAN_POINT('Ctrl Pts',(0.525532604501329,-4.90906733260263,
-2.83425134594813));
#33739=CARTESIAN_POINT('Ctrl Pts',(0.528943702130891,-4.81813466520527,
-2.99175134594813));
#33740=CARTESIAN_POINT('',(0.,-4.81813466520527,-2.99175134594813));
#33741=CARTESIAN_POINT('',(0.,-5.,-2.67675134594813));
#33742=CARTESIAN_POINT('Ctrl Pts',(4.44772342888108,-0.165392353541525,
-5.67801337205715));
#33743=CARTESIAN_POINT('Ctrl Pts',(4.69727026033307,-0.931491616708205,
-5.2357057562419));
#33744=CARTESIAN_POINT('Ctrl Pts',(4.96928012765321,-2.42096936008937,-4.37575538014882));
#33745=CARTESIAN_POINT('Ctrl Pts',(4.78045253748373,-3.81314196223624,-3.57198415354091));
#33746=CARTESIAN_POINT('Ctrl Pts',(4.44772342888108,-4.83460764645847,-2.98224066578724));
#33747=CARTESIAN_POINT('Ctrl Pts',(4.5447241499808,-0.110261569027682,-5.63725117364547));
#33748=CARTESIAN_POINT('Ctrl Pts',(4.7983881862218,-0.881878377310218,-5.19312555764156));
#33749=CARTESIAN_POINT('Ctrl Pts',(5.07815075443906,-2.389498397681,-4.32537672517764));
#33750=CARTESIAN_POINT('Ctrl Pts',(4.8829428649688,-3.79962864594736,-3.50901750660556));
#33751=CARTESIAN_POINT('Ctrl Pts',(4.5447241499808,-4.82687193937677,-2.91411490666184));
#33752=CARTESIAN_POINT('Ctrl Pts',(4.64172487108053,-0.0551307845138397,
-5.59648897523378));
#33753=CARTESIAN_POINT('Ctrl Pts',(4.89950611211053,-0.832265137912234,
-5.15054535904123));
#33754=CARTESIAN_POINT('Ctrl Pts',(5.18702138122492,-2.35802743527264,-4.27499807020645));
#33755=CARTESIAN_POINT('Ctrl Pts',(4.98543319245386,-3.78611532965848,-3.44605085967021));
#33756=CARTESIAN_POINT('Ctrl Pts',(4.64172487108053,-4.81913623229507,-2.84598914753644));
#33757=CARTESIAN_POINT('Ctrl Pts',(4.73872559218025,2.80742846517038E-15,
-5.5557267768221));
#33758=CARTESIAN_POINT('Ctrl Pts',(5.00062403799926,-0.782651898514247,
-5.10796516044089));
#33759=CARTESIAN_POINT('Ctrl Pts',(5.29589200801077,-2.32655647286427,-4.22461941523526));
#33760=CARTESIAN_POINT('Ctrl Pts',(5.08792351993893,-3.7726020133696,-3.38308421273486));
#33761=CARTESIAN_POINT('Ctrl Pts',(4.73872559218025,-4.81140052521337,-2.77786338841105));
#33762=CARTESIAN_POINT('Ctrl Pts',(4.45307670887188,-4.81813292344042,-2.99175235155653));
#33763=CARTESIAN_POINT('Ctrl Pts',(4.78160975160098,-3.8045770857894,-3.57692908726306));
#33764=CARTESIAN_POINT('Ctrl Pts',(4.96786706546316,-2.42067099411741,-4.37592764182305));
#33765=CARTESIAN_POINT('Ctrl Pts',(4.69893917059593,-0.940653225099448,
-5.230416299171));
#33766=CARTESIAN_POINT('Ctrl Pts',(4.45307570990783,-0.181866974811239,
-5.66850174503229));
#33767=CARTESIAN_POINT('Origin',(0.,4.90906733260264,2.83425134594813));
#33768=CARTESIAN_POINT('',(0.528943702130891,5.,2.67675134594813));
#33769=CARTESIAN_POINT('',(0.528943702130891,4.81813466520527,2.99175134594813));
#33770=CARTESIAN_POINT('Ctrl Pts',(0.528943702130891,5.,2.67675134594813));
#33771=CARTESIAN_POINT('Ctrl Pts',(0.525532604501329,4.90906733260263,2.83425134594813));
#33772=CARTESIAN_POINT('Ctrl Pts',(0.528943702130891,4.81813466520527,2.99175134594813));
#33773=CARTESIAN_POINT('',(0.,4.81813466520527,2.99175134594813));
#33774=CARTESIAN_POINT('',(0.,5.,2.67675134594813));
#33775=CARTESIAN_POINT('Origin',(0.,-1.37043154602168E-15,-5.66850269189626));
#33776=CARTESIAN_POINT('',(0.528943702130891,-0.181865334794732,-5.66850269189626));
#33777=CARTESIAN_POINT('',(0.528943702130891,0.181865334794731,-5.66850269189626));
#33778=CARTESIAN_POINT('Ctrl Pts',(0.528943702130891,-0.181865334794732,
-5.66850269189626));
#33779=CARTESIAN_POINT('Ctrl Pts',(0.525532604501329,3.46944695195361E-17,
-5.66850269189626));
#33780=CARTESIAN_POINT('Ctrl Pts',(0.528943702130891,0.181865334794731,
-5.66850269189626));
#33781=CARTESIAN_POINT('',(0.,0.18186533479473,-5.66850269189626));
#33782=CARTESIAN_POINT('',(0.,-0.181865334794733,-5.66850269189626));
#33783=CARTESIAN_POINT('Origin',(0.,4.90906733260263,-2.83425134594813));
#33784=CARTESIAN_POINT('',(0.528943702130891,4.81813466520527,-2.99175134594813));
#33785=CARTESIAN_POINT('',(0.52894370213089,5.,-2.67675134594813));
#33786=CARTESIAN_POINT('Ctrl Pts',(0.528943702130891,4.81813466520527,-2.99175134594813));
#33787=CARTESIAN_POINT('Ctrl Pts',(0.525532604501329,4.90906733260263,-2.83425134594813));
#33788=CARTESIAN_POINT('Ctrl Pts',(0.52894370213089,5.,-2.67675134594813));
#33789=CARTESIAN_POINT('',(0.,5.,-2.67675134594813));
#33790=CARTESIAN_POINT('',(0.,4.81813466520527,-2.99175134594813));
#33791=CARTESIAN_POINT('Origin',(0.,5.,2.88675134594813));
#33792=CARTESIAN_POINT('Ctrl Pts',(0.528943702130891,4.81813466520527,2.99175134594813));
#33793=CARTESIAN_POINT('Ctrl Pts',(-0.209998305499054,2.5,4.33012701892219));
#33794=CARTESIAN_POINT('Ctrl Pts',(0.528943702130891,0.181865334794731,
5.66850269189626));
#33795=CARTESIAN_POINT('Origin',(0.,5.,-2.88675134594813));
#33796=CARTESIAN_POINT('Ctrl Pts',(0.52894370213089,5.,-2.67675134594813));
#33797=CARTESIAN_POINT('Ctrl Pts',(-0.209998305499052,5.,-5.55111512312578E-16));
#33798=CARTESIAN_POINT('Ctrl Pts',(0.528943702130891,5.,2.67675134594813));
#33799=CARTESIAN_POINT('Origin',(0.,-1.06057523872491E-15,-5.77350269189626));
#33800=CARTESIAN_POINT('Ctrl Pts',(0.528943702130891,0.181865334794731,
-5.66850269189626));
#33801=CARTESIAN_POINT('Ctrl Pts',(-0.209998305499051,2.5,-4.33012701892219));
#33802=CARTESIAN_POINT('Ctrl Pts',(0.528943702130891,4.81813466520527,-2.99175134594813));
#33803=CARTESIAN_POINT('Origin',(0.377062317719749,0.,0.));
#33804=CARTESIAN_POINT('',(0.136226494320606,-5.,-3.68823841089113E-16));
#33805=CARTESIAN_POINT('',(0.377062317719749,-5.41175134594813,-6.62748396359676E-16));
#33806=CARTESIAN_POINT('Ctrl Pts',(0.528943702130891,-5.,2.67675134594813));
#33807=CARTESIAN_POINT('Ctrl Pts',(0.136226494320606,-5.,1.25416837769224));
#33808=CARTESIAN_POINT('Ctrl Pts',(0.136226494320606,-5.,-1.25324282604549E-16));
#33809=CARTESIAN_POINT('Ctrl Pts',(0.528943702130891,-0.181865334794732,
5.66850269189626));
#33810=CARTESIAN_POINT('Ctrl Pts',(-0.209998305499052,-2.5,4.33012701892219));
#33811=CARTESIAN_POINT('Ctrl Pts',(0.528943702130891,-4.81813466520527,
2.99175134594813));
#33812=CARTESIAN_POINT('Ctrl Pts',(0.528943702130891,-4.81813466520527,
-2.99175134594813));
#33813=CARTESIAN_POINT('Ctrl Pts',(-0.209998305499052,-2.5,-4.33012701892219));
#33814=CARTESIAN_POINT('Ctrl Pts',(0.528943702130891,-0.181865334794732,
-5.66850269189626));
#33815=CARTESIAN_POINT('Ctrl Pts',(0.136226494320606,-5.,-1.25324282604549E-16));
#33816=CARTESIAN_POINT('Ctrl Pts',(0.136226494320606,-5.,-1.25416837769224));
#33817=CARTESIAN_POINT('Ctrl Pts',(0.52894370213089,-5.,-2.67675134594813));
#33818=CARTESIAN_POINT('Origin',(0.,-5.,-2.88675134594813));
#33819=CARTESIAN_POINT('Origin',(0.,-5.,2.88675134594813));
#33820=CARTESIAN_POINT('Origin',(0.,3.53525079574969E-16,5.77350269189626));
#33821=CARTESIAN_POINT('',(0.,0.,0.));
#33822=CARTESIAN_POINT('Origin',(0.,0.,0.));
#33823=CARTESIAN_POINT('',(-1.22464679914735E-16,-1.49975978266186E-32,
2.));
#33824=CARTESIAN_POINT('',(-1.22464679914735E-16,-1.49975978266186E-32,
-2.));
#33825=CARTESIAN_POINT('Origin',(0.,0.,0.));
#33826=CARTESIAN_POINT('',(0.,0.,0.));
#33827=CARTESIAN_POINT('Ctrl Pts',(0.508591862447781,1.64562043801211,-0.0261324580079617));
#33828=CARTESIAN_POINT('Ctrl Pts',(0.528271024599208,1.6452737407805,0.161128837931408));
#33829=CARTESIAN_POINT('Ctrl Pts',(0.567647573513685,1.58281094560678,0.524492831752905));
#33830=CARTESIAN_POINT('Ctrl Pts',(0.645996560435206,1.22365592193525,1.1787804941138));
#33831=CARTESIAN_POINT('Ctrl Pts',(0.743073641882897,0.410281924307437,
1.68766009875447));
#33832=CARTESIAN_POINT('Ctrl Pts',(0.858352417401347,-0.724396860085975,
1.55831173688398));
#33833=CARTESIAN_POINT('Ctrl Pts',(0.972375295448021,-1.52098532662473,
0.758217612597792));
#33834=CARTESIAN_POINT('Ctrl Pts',(1.08519171777668,-1.64409811634449,-0.352032188510366));
#33835=CARTESIAN_POINT('Ctrl Pts',(1.19681996654867,-1.05450947578872,-1.28675893283186));
#33836=CARTESIAN_POINT('Ctrl Pts',(1.30730161177351,-0.0208333311052113,
-1.64663068201152));
#33837=CARTESIAN_POINT('Ctrl Pts',(1.40452364629174,0.886236470079679,-1.32621345051066));
#33838=CARTESIAN_POINT('Ctrl Pts',(1.48890750188156,1.38959463750653,-0.691912415510853));
#33839=CARTESIAN_POINT('Ctrl Pts',(1.56078188611823,1.54308896603543,-0.0198177610475133));
#33840=CARTESIAN_POINT('Ctrl Pts',(1.63221817171176,1.38983552550406,0.647948130516392));
#33841=CARTESIAN_POINT('Ctrl Pts',(1.70323404319384,0.964738946565908,1.1812205675546));
#33842=CARTESIAN_POINT('Ctrl Pts',(1.77384798276294,0.354991450441324,1.47260961294232));
#33843=CARTESIAN_POINT('Ctrl Pts',(1.86748993119896,-0.546099502039117,
1.47825694934893));
#33844=CARTESIAN_POINT('Ctrl Pts',(1.98363667823136,-1.48203264186415,0.7293081873873));
#33845=CARTESIAN_POINT('Ctrl Pts',(2.09871900316068,-1.48120258062414,-0.462340692211473));
#33846=CARTESIAN_POINT('Ctrl Pts',(2.19023826573612,-0.927379733426102,
-1.14481302651884));
#33847=CARTESIAN_POINT('Ctrl Pts',(2.2814255547235,-0.141378759287938,-1.52891931607764));
#33848=CARTESIAN_POINT('Ctrl Pts',(2.39484749559815,1.00382275253285,-1.27061478852019));
#33849=CARTESIAN_POINT('Ctrl Pts',(2.53025681997088,1.60865186335246,-0.00254459019504153));
#33850=CARTESIAN_POINT('Ctrl Pts',(2.64269039045238,1.10418776314993,1.04117197496908));
#33851=CARTESIAN_POINT('Ctrl Pts',(2.73249952801582,0.322974585676589,1.41105820876749));
#33852=CARTESIAN_POINT('Ctrl Pts',(2.7998141074244,-0.32110895921182,1.41232437949226));
#33853=CARTESIAN_POINT('Ctrl Pts',(2.86711382621074,-0.903428721470414,
1.13164638734841));
#33854=CARTESIAN_POINT('Ctrl Pts',(2.93442516377676,-1.30601623783849,0.626923391067463));
#33855=CARTESIAN_POINT('Ctrl Pts',(3.00177556402078,-1.44931171614156,-0.00280700337714968));
#33856=CARTESIAN_POINT('Ctrl Pts',(3.08042754178598,-1.28252605621248,-0.73905091180395));
#33857=CARTESIAN_POINT('Ctrl Pts',(3.17046965462109,-0.654511755766728,
-1.3704712298758));
#33858=CARTESIAN_POINT('Ctrl Pts',(3.27206448378161,0.346719679199525,-1.483704431146));
#33859=CARTESIAN_POINT('Ctrl Pts',(3.3740442463093,1.20102786916375,-0.946430056825302));
#33860=CARTESIAN_POINT('Ctrl Pts',(3.47649477143674,1.53732148053407,0.0107120740773195));
#33861=CARTESIAN_POINT('Ctrl Pts',(3.57949954098879,1.20134163447082,0.973667458417707));
#33862=CARTESIAN_POINT('Ctrl Pts',(3.68313928551533,0.333095090941954,1.52059902024328));
#33863=CARTESIAN_POINT('Ctrl Pts',(3.78749120379714,-0.693842597912142,
1.40614340263662));
#33864=CARTESIAN_POINT('Ctrl Pts',(3.89262893585172,-1.43094857905026,0.670971912346831));
#33865=CARTESIAN_POINT('Ctrl Pts',(3.99862203011025,-1.5499543985351,-0.371794281933162));
#33866=CARTESIAN_POINT('Ctrl Pts',(4.10553567293418,-0.988090997030439,
-1.26903707993744));
#33867=CARTESIAN_POINT('Ctrl Pts',(4.21343045112327,0.0197202801860453,
-1.62347464599002));
#33868=CARTESIAN_POINT('Ctrl Pts',(4.32236196180067,1.03832038776908,-1.26894288895586));
#33869=CARTESIAN_POINT('Ctrl Pts',(4.43238051112357,1.61925828890368,-0.34739423883176));
#33870=CARTESIAN_POINT('Ctrl Pts',(4.54353062752128,1.4989897755625,0.74620181404568));
#33871=CARTESIAN_POINT('Ctrl Pts',(4.65585125526312,0.71351870218781,1.53444845290457));
#33872=CARTESIAN_POINT('Ctrl Pts',(4.75676135685292,-0.279697500338493,
1.64729603227415));
#33873=CARTESIAN_POINT('Ctrl Pts',(4.84585493867587,-1.04780204615629,1.27474307821934));
#33874=CARTESIAN_POINT('Ctrl Pts',(4.94841313843452,-1.66845031883017,0.508931034591464));
#33875=CARTESIAN_POINT('Ctrl Pts',(5.07800659502253,-1.67475443904525,-0.829467776745351));
#33876=CARTESIAN_POINT('Ctrl Pts',(5.23577771702336,-0.399579932550961,
-1.85373353020478));
#33877=CARTESIAN_POINT('Ctrl Pts',(5.39581269472486,1.21472097060722,-1.48922395511139));
#33878=CARTESIAN_POINT('Ctrl Pts',(5.55809610080897,1.95203227446324,0.0217272724024816));
#33879=CARTESIAN_POINT('Ctrl Pts',(5.70888367040444,1.27533356599845,1.42745494534175));
#33880=CARTESIAN_POINT('Ctrl Pts',(5.84753617842438,-0.0234051752573978,
1.87960329280061));
#33881=CARTESIAN_POINT('Ctrl Pts',(5.9735033792588,-1.2000636353636,1.47084402209574));
#33882=CARTESIAN_POINT('Ctrl Pts',(6.10061934653175,-1.87205652425054,0.4054527917675));
#33883=CARTESIAN_POINT('Ctrl Pts',(6.22882892874595,-1.73128184695155,-0.856020464879398));
#33884=CARTESIAN_POINT('Ctrl Pts',(6.35811249074499,-0.82796691613823,-1.76256406416465));
#33885=CARTESIAN_POINT('Ctrl Pts',(6.48835538046169,0.454518312141212,-1.90827828922266));
#33886=CARTESIAN_POINT('Ctrl Pts',(6.59776527270895,1.37009311469038,-1.33377327146165));
#33887=CARTESIAN_POINT('Ctrl Pts',(6.68557306476182,1.77276616876359,-0.600525447669764));
#33888=CARTESIAN_POINT('Ctrl Pts',(6.72979494253028,1.84279755540219,-0.192431284750887));
#33889=CARTESIAN_POINT('Ctrl Pts',(6.75172308477496,1.84318387398818,0.016230664703078));
#33890=CARTESIAN_POINT('Ctrl Pts',(0.509580047382347,1.70171160283773,-0.0261324580079617));
#33891=CARTESIAN_POINT('Ctrl Pts',(0.529895087764518,1.70135370303456,0.167179673868041));
#33892=CARTESIAN_POINT('Ctrl Pts',(0.570639757970856,1.63675411705557,0.543184963069467));
#33893=CARTESIAN_POINT('Ctrl Pts',(0.6516200225759,1.26545922887677,1.21943960034875));
#33894=CARTESIAN_POINT('Ctrl Pts',(0.752012920500956,0.424415974257467,
1.74584191963726));
#33895=CARTESIAN_POINT('Ctrl Pts',(0.871203035093005,-0.748901033499195,
1.61196056324099));
#33896=CARTESIAN_POINT('Ctrl Pts',(0.989080507646655,-1.57236986743728,
0.784770914561726));
#33897=CARTESIAN_POINT('Ctrl Pts',(1.10566189091232,-1.69947969245876,-0.362632153218937));
#33898=CARTESIAN_POINT('Ctrl Pts',(1.22095215672461,-1.09039676853272,-1.32796705536343));
#33899=CARTESIAN_POINT('Ctrl Pts',(1.33497129130756,-0.0235221960857565,
-1.69919666569563));
#33900=CARTESIAN_POINT('Ctrl Pts',(1.43521215485341,0.911646464020701,-1.36863402635081));
#33901=CARTESIAN_POINT('Ctrl Pts',(1.52213389548391,1.43007830855258,-0.715200055347309));
#33902=CARTESIAN_POINT('Ctrl Pts',(1.59610957693942,1.58797356382673,-0.0234496931959115));
#33903=CARTESIAN_POINT('Ctrl Pts',(1.6695643364048,1.43030938586697,0.663167430554008));
#33904=CARTESIAN_POINT('Ctrl Pts',(1.74251566986873,0.993555991276766,1.21088878338602));
#33905=CARTESIAN_POINT('Ctrl Pts',(1.81497296241828,0.367875249236745,1.50980906152487));
#33906=CARTESIAN_POINT('Ctrl Pts',(1.91095320023966,-0.555718724718245,
1.51541429690618));
#33907=CARTESIAN_POINT('Ctrl Pts',(2.02977137858219,-1.51271899954516,0.748724773148181));
#33908=CARTESIAN_POINT('Ctrl Pts',(2.14718490518103,-1.51104304623224,-0.466989387116428));
#33909=CARTESIAN_POINT('Ctrl Pts',(2.24034153374774,-0.94726476473438,-1.16142922577992));
#33910=CARTESIAN_POINT('Ctrl Pts',(2.33300573809692,-0.148443790584567,
-1.5516251873687));
#33911=CARTESIAN_POINT('Ctrl Pts',(2.44801880375704,1.01237692380644,-1.28879026893535));
#33912=CARTESIAN_POINT('Ctrl Pts',(2.58481878669611,1.62223628112757,-0.00735339085508992));
#33913=CARTESIAN_POINT('Ctrl Pts',(2.69799779409897,1.11364043446412,1.04273258659252));
#33914=CARTESIAN_POINT('Ctrl Pts',(2.78815431916423,0.329470398073438,1.41374437778883));
#33915=CARTESIAN_POINT('Ctrl Pts',(2.85560391946039,-0.315812807091245,
1.41487913006738));
#33916=CARTESIAN_POINT('Ctrl Pts',(2.92290913292631,-0.898041393277587,
1.13407835691753));
#33917=CARTESIAN_POINT('Ctrl Pts',(2.99010748782479,-1.29975039474633,0.630211173964469));
#33918=CARTESIAN_POINT('Ctrl Pts',(3.05720153737446,-1.44237298019696,0.00291322106573988));
#33919=CARTESIAN_POINT('Ctrl Pts',(3.13540758721451,-1.27637311566389,-0.729048078712233));
#33920=CARTESIAN_POINT('Ctrl Pts',(3.22474166887994,-0.653103075230279,
-1.35515277979788));
#33921=CARTESIAN_POINT('Ctrl Pts',(3.32529053184942,0.337558356289205,-1.46669075353571));
#33922=CARTESIAN_POINT('Ctrl Pts',(3.42590699610091,1.18013302272422,-0.936320642038885));
#33923=CARTESIAN_POINT('Ctrl Pts',(3.52675591022479,1.5106801904221,0.00578391821411416));
#33924=CARTESIAN_POINT('Ctrl Pts',(3.62789543596507,1.1804735150479,0.950962905372855));
#33925=CARTESIAN_POINT('Ctrl Pts',(3.72942248398239,0.329909659532609,1.48630965540244));
#33926=CARTESIAN_POINT('Ctrl Pts',(3.83142370458731,-0.673643861606902,
1.37409910302327));
#33927=CARTESIAN_POINT('Ctrl Pts',(3.93398592718664,-1.39230980841848,0.656853426449074));
#33928=CARTESIAN_POINT('Ctrl Pts',(4.03719172387346,-1.50786192508977,-0.358317467730407));
#33929=CARTESIAN_POINT('Ctrl Pts',(4.14112075232382,-0.961565622810986,
-1.23019350319165));
#33930=CARTESIAN_POINT('Ctrl Pts',(4.24584932913355,0.0165600109717206,
-1.57393537894064));
#33931=CARTESIAN_POINT('Ctrl Pts',(4.35144915285955,1.00374162047219,-1.23012207438448));
#33932=CARTESIAN_POINT('Ctrl Pts',(4.4579909264812,1.56609007503267,-0.337790096423364));
#33933=CARTESIAN_POINT('Ctrl Pts',(4.56551149543496,1.44958631126263,0.719976289482437));
#33934=CARTESIAN_POINT('Ctrl Pts',(4.67411908241366,0.69021449004645,1.48194813108531));
#33935=CARTESIAN_POINT('Ctrl Pts',(4.77164000284681,-0.26949798097472,1.59091301338937));
#33936=CARTESIAN_POINT('Ctrl Pts',(4.85771048721972,-1.01144589727057,1.23104757178239));
#33937=CARTESIAN_POINT('Ctrl Pts',(4.9567809680996,-1.61090774880558,0.491362209635852));
#33938=CARTESIAN_POINT('Ctrl Pts',(5.08196285876115,-1.61704639101494,-0.801332081949465));
#33939=CARTESIAN_POINT('Ctrl Pts',(5.23440617825647,-0.385186946102618,
-1.79103900031212));
#33940=CARTESIAN_POINT('Ctrl Pts',(5.38912164940439,1.17539727930777,-1.43897710296556));
#33941=CARTESIAN_POINT('Ctrl Pts',(5.54614784502495,1.88913047177666,0.0227340869851706));
#33942=CARTESIAN_POINT('Ctrl Pts',(5.69223084261495,1.23407058093322,1.38466393862149));
#33943=CARTESIAN_POINT('Ctrl Pts',(5.82670511437593,-0.0254194746735188,
1.82344694793182));
#33944=CARTESIAN_POINT('Ctrl Pts',(5.94902331756535,-1.1680230768833,1.42680551782825));
#33945=CARTESIAN_POINT('Ctrl Pts',(6.07261244268437,-1.82162602449473,0.391140168157498));
#33946=CARTESIAN_POINT('Ctrl Pts',(6.19744218367146,-1.68489344120707,-0.837072796063665));
#33947=CARTESIAN_POINT('Ctrl Pts',(6.32349906024936,-0.804352968952716,
-1.72132362315681));
#33948=CARTESIAN_POINT('Ctrl Pts',(6.45070645344015,0.448136825520351,-1.86394181546585));
#33949=CARTESIAN_POINT('Ctrl Pts',(6.55771675748864,1.343944695716,-1.30238352555007));
#33950=CARTESIAN_POINT('Ctrl Pts',(6.64375918572647,1.73853556054087,-0.583881007842722));
#33951=CARTESIAN_POINT('Ctrl Pts',(6.68709903227955,1.80719676573851,-0.1839314494448));
#33952=CARTESIAN_POINT('Ctrl Pts',(6.70861691504104,1.80757585658667,0.0208265877402715));
#33953=CARTESIAN_POINT('Ctrl Pts',(0.48473626150267,1.77644942930338,-0.0233832711793042));
#33954=CARTESIAN_POINT('Ctrl Pts',(0.505893844496287,1.7760766860232,0.177946255954152));
#33955=CARTESIAN_POINT('Ctrl Pts',(0.548463328130588,1.70860250247314,0.570776926736889));
#33956=CARTESIAN_POINT('Ctrl Pts',(0.632982327171215,1.32101158554047,1.27654377010548));
#33957=CARTESIAN_POINT('Ctrl Pts',(0.737996501360194,0.441739014073499,
1.82746202052102));
#33958=CARTESIAN_POINT('Ctrl Pts',(0.862723494828206,-0.786157377851955,
1.68745064871946));
#33959=CARTESIAN_POINT('Ctrl Pts',(0.986209664727694,-1.64882413818832,
0.821304842815863));
#33960=CARTESIAN_POINT('Ctrl Pts',(1.10839876372818,-1.78218917322355,-0.381247653647888));
#33961=CARTESIAN_POINT('Ctrl Pts',(1.22928857352045,-1.14366016506855,-1.39342331335522));
#33962=CARTESIAN_POINT('Ctrl Pts',(1.34886146417612,-0.0248717421322719,
-1.78277108349345));
#33963=CARTESIAN_POINT('Ctrl Pts',(1.45397742207399,0.955759686067741,-1.4361457574584));
#33964=CARTESIAN_POINT('Ctrl Pts',(1.54509991200394,1.49922256563711,-0.751131218932962));
#33965=CARTESIAN_POINT('Ctrl Pts',(1.62262212832639,1.66468393757921,-0.0261951730747789));
#33966=CARTESIAN_POINT('Ctrl Pts',(1.69956649110401,1.49950125883268,0.693032382528641));
#33967=CARTESIAN_POINT('Ctrl Pts',(1.77593637879585,1.04223323460681,1.26643212720561));
#33968=CARTESIAN_POINT('Ctrl Pts',(1.85174001831755,0.387640963552032,1.57911778202419));
#33969=CARTESIAN_POINT('Ctrl Pts',(1.95206329984898,-0.577882239813857,
1.58491583806782));
#33970=CARTESIAN_POINT('Ctrl Pts',(2.07609288529357,-1.57652280363707,0.784118879423183));
#33971=CARTESIAN_POINT('Ctrl Pts',(2.19835334034983,-1.57411269447054,-0.481987546861393));
#33972=CARTESIAN_POINT('Ctrl Pts',(2.29515759309052,-0.988081044302533,
-1.20354579776995));
#33973=CARTESIAN_POINT('Ctrl Pts',(2.39131513088785,-0.158981373237876,
-1.6083713901134));
#33974=CARTESIAN_POINT('Ctrl Pts',(2.5103164166735,1.04239264391016,-1.33544690779909));
#33975=CARTESIAN_POINT('Ctrl Pts',(2.65138524018481,1.67017090611041,-0.0133144094548457));
#33976=CARTESIAN_POINT('Ctrl Pts',(2.76761689590905,1.14685339948012,1.06483740920086));
#33977=CARTESIAN_POINT('Ctrl Pts',(2.85989151047589,0.344054458745719,1.44437130805655));
#33978=CARTESIAN_POINT('Ctrl Pts',(2.92876498103789,-0.315007838050914,
1.44542580052931));
#33979=CARTESIAN_POINT('Ctrl Pts',(2.99733123089316,-0.908178327495592,
1.1591356196893));
#33980=CARTESIAN_POINT('Ctrl Pts',(3.065609203041,-1.31633070800262,0.646932225733396));
#33981=CARTESIAN_POINT('Ctrl Pts',(3.13363492285534,-1.46075866519691,0.0108009638378416));
#33982=CARTESIAN_POINT('Ctrl Pts',(3.2127246664228,-1.29265108627793,-0.729519994292884));
#33983=CARTESIAN_POINT('Ctrl Pts',(3.30276107775906,-0.663900215810431,
-1.36029592969158));
#33984=CARTESIAN_POINT('Ctrl Pts',(3.40366000172583,0.330744582477941,-1.47158912535297));
#33985=CARTESIAN_POINT('Ctrl Pts',(3.50428991474366,1.17315483841855,-0.940484753739533));
#33986=CARTESIAN_POINT('Ctrl Pts',(3.60471206445919,1.50180382114359,-0.00182149644391336));
#33987=CARTESIAN_POINT('Ctrl Pts',(3.70503499179928,1.1735346580546,0.935792533952136));
#33988=CARTESIAN_POINT('Ctrl Pts',(3.8053502869075,0.332515303599265,1.46435790052267));
#33989=CARTESIAN_POINT('Ctrl Pts',(3.90575276069741,-0.655532733693565,
1.35324201618498));
#33990=CARTESIAN_POINT('Ctrl Pts',(4.0063357525127,-1.36010254886635,0.649193189923515));
#33991=CARTESIAN_POINT('Ctrl Pts',(4.10719217500436,-1.47247077545791,-0.343223377561497));
#33992=CARTESIAN_POINT('Ctrl Pts',(4.20841335510511,-0.939776138769746,
-1.1923257631531));
#33993=CARTESIAN_POINT('Ctrl Pts',(4.31008881701827,0.0102721264493911,
-1.52564233507173));
#33994=CARTESIAN_POINT('Ctrl Pts',(4.41230607006117,0.965941125693951,-1.19227951792117));
#33995=CARTESIAN_POINT('Ctrl Pts',(4.51514840136008,1.50849130946414,-0.330439751053724));
#33996=CARTESIAN_POINT('Ctrl Pts',(4.61870840436037,1.39590489437915,0.688474310705198));
#33997=CARTESIAN_POINT('Ctrl Pts',(4.7230411604876,0.665865263436382,1.42037460677782));
#33998=CARTESIAN_POINT('Ctrl Pts',(4.81654767173681,-0.254564879881144,
1.52461360384059));
#33999=CARTESIAN_POINT('Ctrl Pts',(4.89897224099944,-0.965161399415059,
1.17984498732178));
#34000=CARTESIAN_POINT('Ctrl Pts',(4.99374606403791,-1.53863694276043,0.472007785395054));
#34001=CARTESIAN_POINT('Ctrl Pts',(5.11333980190992,-1.54407067005438,-0.763171998627613));
#34002=CARTESIAN_POINT('Ctrl Pts',(5.25878882582696,-0.368307274360266,
-1.70728369755521));
#34003=CARTESIAN_POINT('Ctrl Pts',(5.40629446830278,1.11962985036899,-1.3713425153718));
#34004=CARTESIAN_POINT('Ctrl Pts',(5.55595232991783,1.79986048336761,0.021931639638948));
#34005=CARTESIAN_POINT('Ctrl Pts',(5.69517763482324,1.17545690153292,1.32014816214982));
#34006=CARTESIAN_POINT('Ctrl Pts',(5.82342289422373,-0.0257032202752489,
1.73872373843064));
#34007=CARTESIAN_POINT('Ctrl Pts',(5.94014607560228,-1.11615143607484,1.36030281643229));
#34008=CARTESIAN_POINT('Ctrl Pts',(6.05818632607282,-1.74056421947656,0.371182103626331));
#34009=CARTESIAN_POINT('Ctrl Pts',(6.17754324250935,-1.61002629882336,-0.80318878992352));
#34010=CARTESIAN_POINT('Ctrl Pts',(6.29822057589678,-0.767189384090067,
-1.64997568303796));
#34011=CARTESIAN_POINT('Ctrl Pts',(6.42019478496613,0.433634258784792,-1.78689227136282));
#34012=CARTESIAN_POINT('Ctrl Pts',(6.52293527463248,1.29405210388765,-1.24809073369933));
#34013=CARTESIAN_POINT('Ctrl Pts',(6.60571721409053,1.67365883220886,-0.556808735892081));
#34014=CARTESIAN_POINT('Ctrl Pts',(6.64739595189646,1.73973417470393,-0.172198300266751));
#34015=CARTESIAN_POINT('Ctrl Pts',(6.66814094153175,1.74009964912365,0.0252051062964792));
#34016=CARTESIAN_POINT('Ctrl Pts',(0.381117442983887,1.88549148283562,-0.0122921586285728));
#34017=CARTESIAN_POINT('Ctrl Pts',(0.403532825828836,1.88509658029261,0.20100623325534));
#34018=CARTESIAN_POINT('Ctrl Pts',(0.448799900969048,1.81344132117068,0.618761006536107));
#34019=CARTESIAN_POINT('Ctrl Pts',(0.538679332142541,1.40127335864296,1.36930440711935));
#34020=CARTESIAN_POINT('Ctrl Pts',(0.650838448754394,0.46290690991,1.95859094615097));
#34021=CARTESIAN_POINT('Ctrl Pts',(0.784506730841078,-0.853342453722629,
1.80916959778172));
#34022=CARTESIAN_POINT('Ctrl Pts',(0.917364661912327,-1.78200024295873,
0.877975354207177));
#34023=CARTESIAN_POINT('Ctrl Pts',(1.04926270425752,-1.92666667943644,-0.420181769112088));
#34024=CARTESIAN_POINT('Ctrl Pts',(1.18017007182846,-1.23574698396432,-1.51656075807354));
#34025=CARTESIAN_POINT('Ctrl Pts',(1.31000892844173,-0.0210398826096366,
-1.93988507897714));
#34026=CARTESIAN_POINT('Ctrl Pts',(1.42442730051466,1.0465288908201,-1.56293923922871));
#34027=CARTESIAN_POINT('Ctrl Pts',(1.52378385033388,1.63922012112484,-0.816087647064672));
#34028=CARTESIAN_POINT('Ctrl Pts',(1.60841315506779,1.81993148953039,-0.0247216582983172));
#34029=CARTESIAN_POINT('Ctrl Pts',(1.69249524019256,1.63950112746236,0.761246734592579));
#34030=CARTESIAN_POINT('Ctrl Pts',(1.77602032928508,1.1394414206172,1.38839301192058));
#34031=CARTESIAN_POINT('Ctrl Pts',(1.85897694842633,0.423103070241056,1.73061206360768));
#34032=CARTESIAN_POINT('Ctrl Pts',(1.96881924664199,-0.634001252397349,
1.73700910342183));
#34033=CARTESIAN_POINT('Ctrl Pts',(2.10466048128153,-1.72773172837744,0.859962453630954));
#34034=CARTESIAN_POINT('Ctrl Pts',(2.23852274988566,-1.72484281980162,-0.526238676081834));
#34035=CARTESIAN_POINT('Ctrl Pts',(2.34441167003019,-1.08376675443436,-1.31536550154628));
#34036=CARTESIAN_POINT('Ctrl Pts',(2.44949842855696,-0.177626983089426,
-1.75770921156832));
#34037=CARTESIAN_POINT('Ctrl Pts',(2.57936886683961,1.13316325023126,-1.45907163886627));
#34038=CARTESIAN_POINT('Ctrl Pts',(2.73282739757898,1.81479123414694,-0.0203495029752695));
#34039=CARTESIAN_POINT('Ctrl Pts',(2.85876666181656,1.24669618273856,1.14720091126386));
#34040=CARTESIAN_POINT('Ctrl Pts',(2.95838625405263,0.379992571081585,1.55652976858396));
#34041=CARTESIAN_POINT('Ctrl Pts',(3.03254530339479,-0.329577958511324,
1.55746711909117));
#34042=CARTESIAN_POINT('Ctrl Pts',(3.10615895005409,-0.96625312134884,1.24989533056844));
#34043=CARTESIAN_POINT('Ctrl Pts',(3.17924306329434,-1.40286089813684,0.701552239452624));
#34044=CARTESIAN_POINT('Ctrl Pts',(3.25180396600809,-1.55666651553022,0.0230087966776739));
#34045=CARTESIAN_POINT('Ctrl Pts',(3.33587136562189,-1.37764426396791,-0.763794702731238));
#34046=CARTESIAN_POINT('Ctrl Pts',(3.43113975717292,-0.711774228624347,
-1.4305765381498));
#34047=CARTESIAN_POINT('Ctrl Pts',(3.5372886042444,0.334525637087803,-1.54647218216131));
#34048=CARTESIAN_POINT('Ctrl Pts',(3.64245111618431,1.21419218905581,-0.990566084988547));
#34049=CARTESIAN_POINT('Ctrl Pts',(3.74671900888706,1.55424048357597,-0.0157101568300266));
#34050=CARTESIAN_POINT('Ctrl Pts',(3.85015607940294,1.21467035959478,0.950447047776102));
#34051=CARTESIAN_POINT('Ctrl Pts',(3.9528428913112,0.353239193399766,1.49035956049266));
#34052=CARTESIAN_POINT('Ctrl Pts',(4.05486113278981,-0.650409675441866,
1.37619957489024));
#34053=CARTESIAN_POINT('Ctrl Pts',(4.15629674336446,-1.35992778763908,0.665383226257766));
#34054=CARTESIAN_POINT('Ctrl Pts',(4.25723817727952,-1.47109033257279,-0.327860133764075));
#34055=CARTESIAN_POINT('Ctrl Pts',(4.35777648370015,-0.940986099129111,
-1.17042124327949));
#34056=CARTESIAN_POINT('Ctrl Pts',(4.45800500695589,-0.00418280368968732,
-1.49774982508127));
#34057=CARTESIAN_POINT('Ctrl Pts',(4.5580185838917,0.930328530149581,-1.17045669235878));
#34058=CARTESIAN_POINT('Ctrl Pts',(4.65791431280149,1.45624348325976,-0.332815962728341));
#34059=CARTESIAN_POINT('Ctrl Pts',(4.75778043706964,1.34650681780447,0.649575118733562));
#34060=CARTESIAN_POINT('Ctrl Pts',(4.85772972138868,0.646482048134813,1.3498091217411));
#34061=CARTESIAN_POINT('Ctrl Pts',(4.94672281509739,-0.229473231501492,
1.44804559906066));
#34062=CARTESIAN_POINT('Ctrl Pts',(5.02476069807077,-0.902005151158387,
1.12142327819778));
#34063=CARTESIAN_POINT('Ctrl Pts',(5.11414214502143,-1.44253731235627,0.453534796061982));
#34064=CARTESIAN_POINT('Ctrl Pts',(5.22630308574295,-1.4458617461083,-0.704791410686178));
#34065=CARTESIAN_POINT('Ctrl Pts',(5.36180677972868,-0.349337730909665,
-1.58269217180053));
#34066=CARTESIAN_POINT('Ctrl Pts',(5.49842670840074,1.02827880679783,-1.26994462762035));
#34067=CARTESIAN_POINT('Ctrl Pts',(5.63636184857256,1.65389902289474,0.0147413000363786));
#34068=CARTESIAN_POINT('Ctrl Pts',(5.76418317065839,1.07983232656629,1.20601509187628));
#34069=CARTESIAN_POINT('Ctrl Pts',(5.88159777082462,-0.0199377183914416,
1.58882970514278));
#34070=CARTESIAN_POINT('Ctrl Pts',(5.98828065981164,-1.01646279733448,1.24276792091335));
#34071=CARTESIAN_POINT('Ctrl Pts',(6.09602860027055,-1.58629611726947,0.339763321778818));
#34072=CARTESIAN_POINT('Ctrl Pts',(6.20490847258959,-1.46716302714867,-0.731395319267634));
#34073=CARTESIAN_POINT('Ctrl Pts',(6.31494726512681,-0.698554879731498,
-1.50380945298764));
#34074=CARTESIAN_POINT('Ctrl Pts',(6.42623832876641,0.396834532462986,-1.62857970257978));
#34075=CARTESIAN_POINT('Ctrl Pts',(6.51995917582357,1.18229401202514,-1.1375069093975));
#34076=CARTESIAN_POINT('Ctrl Pts',(6.59569195310362,1.52939583473763,-0.505043507088318));
#34077=CARTESIAN_POINT('Ctrl Pts',(6.63371330954042,1.58973057564736,-0.154190128191221));
#34078=CARTESIAN_POINT('Ctrl Pts',(6.65276483375079,1.59006621547548,0.0270987442288496));
#34079=CARTESIAN_POINT('Ctrl Pts',(0.201836006562775,1.92995577875298,0.00663072711028962));
#34080=CARTESIAN_POINT('Ctrl Pts',(0.224795078860765,1.9295512977723,0.225102712807887));
#34081=CARTESIAN_POINT('Ctrl Pts',(0.271213486384443,1.85616115643364,0.653502313542884));
#34082=CARTESIAN_POINT('Ctrl Pts',(0.363604583187976,1.43267031234386,1.42506685239735));
#34083=CARTESIAN_POINT('Ctrl Pts',(0.479576972855799,0.463331817377741,
2.03555787261258));
#34084=CARTESIAN_POINT('Ctrl Pts',(0.618629625107766,-0.906182013551074,
1.88150617936703));
#34085=CARTESIAN_POINT('Ctrl Pts',(0.757746114284183,-1.87958474430334,
0.9076648120197));
#34086=CARTESIAN_POINT('Ctrl Pts',(0.896706311574424,-2.03342734252753,
-0.459866228468009));
#34087=CARTESIAN_POINT('Ctrl Pts',(1.03546170358268,-1.30229481563026,-1.62266197721363));
#34088=CARTESIAN_POINT('Ctrl Pts',(1.1738866891073,-0.00771058607069546,
-2.07527455834761));
#34089=CARTESIAN_POINT('Ctrl Pts',(1.29655718944891,1.13725471717341,-1.67217948259824));
#34090=CARTESIAN_POINT('Ctrl Pts',(1.40355524104465,1.77588206025209,-0.868120367571199));
#34091=CARTESIAN_POINT('Ctrl Pts',(1.49500705634901,1.97148816005587,-0.0130330893690973));
#34092=CARTESIAN_POINT('Ctrl Pts',(1.58617102513088,1.77617516983714,0.839207774540849));
#34093=CARTESIAN_POINT('Ctrl Pts',(1.67701884112096,1.23252947154644,1.52155822726773));
#34094=CARTESIAN_POINT('Ctrl Pts',(1.76752485196204,0.451082218560783,1.89514370110071));
#34095=CARTESIAN_POINT('Ctrl Pts',(1.88770765503142,-0.705441630270057,
1.90264440991584));
#34096=CARTESIAN_POINT('Ctrl Pts',(2.03695468071265,-1.9081838550806,0.94032766212397));
#34097=CARTESIAN_POINT('Ctrl Pts',(2.18473095478842,-1.90658288368755,-0.589977958798058));
#34098=CARTESIAN_POINT('Ctrl Pts',(2.30198581617906,-1.19676910050402,-1.46411874702317));
#34099=CARTESIAN_POINT('Ctrl Pts',(2.41857160900784,-0.191636557767527,
-1.95505543786729));
#34100=CARTESIAN_POINT('Ctrl Pts',(2.5629888947828,1.2663632428723,-1.62394356863633));
#34101=CARTESIAN_POINT('Ctrl Pts',(2.73407115542912,2.0270803897522,-0.0201760536951305));
#34102=CARTESIAN_POINT('Ctrl Pts',(2.87468753311021,1.39305244293906,1.28367355357035));
#34103=CARTESIAN_POINT('Ctrl Pts',(2.985961186478,0.424866500577374,1.74094181792175));
#34104=CARTESIAN_POINT('Ctrl Pts',(3.06879765074836,-0.367776933829584,
1.74199341254035));
#34105=CARTESIAN_POINT('Ctrl Pts',(3.15100736921607,-1.0788356648381,1.39845630998696));
#34106=CARTESIAN_POINT('Ctrl Pts',(3.23258126027651,-1.56616872509529,0.786326708824376));
#34107=CARTESIAN_POINT('Ctrl Pts',(3.31351914497578,-1.73765670717964,0.0294003216284019));
#34108=CARTESIAN_POINT('Ctrl Pts',(3.40719584708756,-1.53805092823913,-0.847373922431961));
#34109=CARTESIAN_POINT('Ctrl Pts',(3.51317550457446,-0.79697103399377,-1.58892396461612));
#34110=CARTESIAN_POINT('Ctrl Pts',(3.63093975483762,0.364087451579112,-1.71693586757571));
#34111=CARTESIAN_POINT('Ctrl Pts',(3.74726185074701,1.33676222663195,-1.10142473675384));
#34112=CARTESIAN_POINT('Ctrl Pts',(3.86213882267644,1.71071625332947,-0.0269760307547636));
#34113=CARTESIAN_POINT('Ctrl Pts',(3.97559755033401,1.33734506143431,1.03260709602997));
#34114=CARTESIAN_POINT('Ctrl Pts',(4.08766375246609,0.39658526295041,1.62104472468397));
#34115=CARTESIAN_POINT('Ctrl Pts',(4.19837188466259,-0.692552398864759,
1.49604314345822));
#34116=CARTESIAN_POINT('Ctrl Pts',(4.30776281443248,-1.4569519090562,0.728544173315976));
#34117=CARTESIAN_POINT('Ctrl Pts',(4.41588440940527,-1.57476055190118,-0.335612967324715));
#34118=CARTESIAN_POINT('Ctrl Pts',(4.52279088240793,-1.0098659333688,-1.23091885839333));
#34119=CARTESIAN_POINT('Ctrl Pts',(4.62854271946233,-0.0208637422853108,
-1.57498366840481));
#34120=CARTESIAN_POINT('Ctrl Pts',(4.73320651333447,0.956721615277288,-1.23104232731158));
#34121=CARTESIAN_POINT('Ctrl Pts',(4.83685381440459,1.50113720788295,-0.361046551352442));
#34122=CARTESIAN_POINT('Ctrl Pts',(4.93956680559533,1.38675857073312,0.649275822959622));
#34123=CARTESIAN_POINT('Ctrl Pts',(5.04141762750123,0.672155174078915,1.36176713203313));
#34124=CARTESIAN_POINT('Ctrl Pts',(5.13126818486399,-0.212417836755547,
1.45954591835434));
#34125=CARTESIAN_POINT('Ctrl Pts',(5.20944866403957,-0.885934908127286,
1.13191422290279));
#34126=CARTESIAN_POINT('Ctrl Pts',(5.29843130100065,-1.42368217894501,0.466316024045218));
#34127=CARTESIAN_POINT('Ctrl Pts',(5.40904405233104,-1.42383866211022,-0.676135006079988));
#34128=CARTESIAN_POINT('Ctrl Pts',(5.54102654373605,-0.35328520959894,-1.5282437999679));
#34129=CARTESIAN_POINT('Ctrl Pts',(5.67249721216457,0.971590168067238,-1.22370899227755));
#34130=CARTESIAN_POINT('Ctrl Pts',(5.80369886270088,1.5635297180874,-0.00010031995261808));
#34131=CARTESIAN_POINT('Ctrl Pts',(5.92394544959964,1.02078935752518,1.11925283857749));
#34132=CARTESIAN_POINT('Ctrl Pts',(6.03342516804945,-0.00501638868570453,
1.47478640897076));
#34133=CARTESIAN_POINT('Ctrl Pts',(6.13218887234589,-0.92723326445955,1.15337619506912));
#34134=CARTESIAN_POINT('Ctrl Pts',(6.23127805234855,-1.45037454055268,0.322285760023574));
#34135=CARTESIAN_POINT('Ctrl Pts',(6.33081386970904,-1.34051708598646,-0.656728344800009));
#34136=CARTESIAN_POINT('Ctrl Pts',(6.43084535343457,-0.641085133745283,
-1.35854714858885));
#34137=CARTESIAN_POINT('Ctrl Pts',(6.53157235049208,0.350142317022017,-1.47042556616477));
#34138=CARTESIAN_POINT('Ctrl Pts',(6.61595803451021,1.05760233194793,-1.02813235011111));
#34139=CARTESIAN_POINT('Ctrl Pts',(6.68412403526691,1.36966491076677,-0.458766422246885));
#34140=CARTESIAN_POINT('Ctrl Pts',(6.7181331127701,1.42366222550641,-0.144933967556013));
#34141=CARTESIAN_POINT('Ctrl Pts',(6.73533237399976,1.42396523313032,0.0187292984563378));
#34142=CARTESIAN_POINT('Ctrl Pts',(0.0055986102182942,1.7786917886362,0.0269731300457806));
#34143=CARTESIAN_POINT('Ctrl Pts',(0.0269030153260128,1.77831645872047,
0.229699774553832));
#34144=CARTESIAN_POINT('Ctrl Pts',(0.0697170102000981,1.71067986121277,
0.624862173397813));
#34145=CARTESIAN_POINT('Ctrl Pts',(0.155518742768547,1.31788830620784,1.34153507286603));
#34146=CARTESIAN_POINT('Ctrl Pts',(0.263771619458144,0.413530357430306,
1.91245230228306));
#34147=CARTESIAN_POINT('Ctrl Pts',(0.394742448193518,-0.876433246166832,
1.76940441846535));
#34148=CARTESIAN_POINT('Ctrl Pts',(0.526895266046311,-1.8025697956283,0.845508368090719));
#34149=CARTESIAN_POINT('Ctrl Pts',(0.6600878321834,-1.95199027993901,-0.464994289895076));
#34150=CARTESIAN_POINT('Ctrl Pts',(0.794281538807695,-1.24660356207781,
-1.59065630973919));
#34151=CARTESIAN_POINT('Ctrl Pts',(0.929381540394946,0.0161873708636046,
-2.03437466461124));
#34152=CARTESIAN_POINT('Ctrl Pts',(1.05020992338902,1.14459879547428,-1.63901960444341));
#34153=CARTESIAN_POINT('Ctrl Pts',(1.1564113362939,1.77908325177254,-0.841350702215082));
#34154=CARTESIAN_POINT('Ctrl Pts',(1.24774422943565,1.97499565916099,0.0124643607619269));
#34155=CARTESIAN_POINT('Ctrl Pts',(1.33935066447099,1.77932241292938,0.868971342433958));
#34156=CARTESIAN_POINT('Ctrl Pts',(1.43120343117607,1.23018382091282,1.55925189286057));
#34157=CARTESIAN_POINT('Ctrl Pts',(1.52327258476988,0.435406173219395,1.93975522009938));
#34158=CARTESIAN_POINT('Ctrl Pts',(1.64628334757985,-0.747955935764237,
1.94844299211941));
#34159=CARTESIAN_POINT('Ctrl Pts',(1.80043942830411,-1.99282994775571,0.957661401566267));
#34160=CARTESIAN_POINT('Ctrl Pts',(1.95492260956612,-1.99542728549998,-0.64185356411705));
#34161=CARTESIAN_POINT('Ctrl Pts',(2.07857944637526,-1.2473256436638,-1.5645532630108));
#34162=CARTESIAN_POINT('Ctrl Pts',(2.20224026315262,-0.181801586351347,
-2.08583346026664));
#34163=CARTESIAN_POINT('Ctrl Pts',(2.35676056686682,1.37874519474033,-1.73564260477601));
#34164=CARTESIAN_POINT('Ctrl Pts',(2.54182526832312,2.20609106907775,-0.00268827228171362));
#34165=CARTESIAN_POINT('Ctrl Pts',(2.69555119442166,1.51605336872507,1.42417233727536));
#34166=CARTESIAN_POINT('Ctrl Pts',(2.81811658390143,0.449775260975512,1.92865218693433));
#34167=CARTESIAN_POINT('Ctrl Pts',(2.90980425579794,-0.427472809728478,
1.93018337506389));
#34168=CARTESIAN_POINT('Ctrl Pts',(3.0012257313044,-1.21838376850936,1.54862371335145));
#34169=CARTESIAN_POINT('Ctrl Pts',(3.09235597402077,-1.76311410577726,0.865082768968332));
#34170=CARTESIAN_POINT('Ctrl Pts',(3.18316203145471,-1.95590236528654,0.0159781933622966));
#34171=CARTESIAN_POINT('Ctrl Pts',(3.28869781156922,-1.73151158460335,-0.971832032847293));
#34172=CARTESIAN_POINT('Ctrl Pts',(3.40869099291695,-0.893323402037981,
-1.81213480121132));
#34173=CARTESIAN_POINT('Ctrl Pts',(3.5427667337023,0.428303253574616,-1.95909052352705));
#34174=CARTESIAN_POINT('Ctrl Pts',(3.67583348666243,1.54154498477032,-1.25584048760503));
#34175=CARTESIAN_POINT('Ctrl Pts',(3.80783173039662,1.97204661692226,-0.0216508987713537));
#34176=CARTESIAN_POINT('Ctrl Pts',(3.93868718175276,1.5421657385633,1.20058177185902));
#34177=CARTESIAN_POINT('Ctrl Pts',(4.06833893810746,0.454165564969672,1.88182985373663));
#34178=CARTESIAN_POINT('Ctrl Pts',(4.19673100805262,-0.808925769374989,
1.73731835455084));
#34179=CARTESIAN_POINT('Ctrl Pts',(4.32381422461611,-1.6971140366654,0.845943606081325));
#34180=CARTESIAN_POINT('Ctrl Pts',(4.44954593492418,-1.83423268382295,-0.391455693145508));
#34181=CARTESIAN_POINT('Ctrl Pts',(4.57389042061536,-1.17720068138488,-1.43272620490813));
#34182=CARTESIAN_POINT('Ctrl Pts',(4.69681904943983,-0.0275512378076592,
-1.83246320358028));
#34183=CARTESIAN_POINT('Ctrl Pts',(4.81831031197903,1.10702608934609,-1.43289530427454));
#34184=CARTESIAN_POINT('Ctrl Pts',(4.9383507013174,1.73706127318637,-0.425069901136755));
#34185=CARTESIAN_POINT('Ctrl Pts',(5.05692960886477,1.60431828004724,0.741229170655166));
#34186=CARTESIAN_POINT('Ctrl Pts',(5.17405567081681,0.78196805313534,1.55992384717266));
#34187=CARTESIAN_POINT('Ctrl Pts',(5.27687879209034,-0.230347348735859,
1.67087959864774));
#34188=CARTESIAN_POINT('Ctrl Pts',(5.36591877038285,-0.997165099457179,
1.29747944846882));
#34189=CARTESIAN_POINT('Ctrl Pts',(5.46683882163731,-1.60675724871016,0.542112054460348));
#34190=CARTESIAN_POINT('Ctrl Pts',(5.59143208581872,-1.60417349359218,-0.744753029658688));
#34191=CARTESIAN_POINT('Ctrl Pts',(5.7385327841038,-0.408499051200149,-1.69141896776007));
#34192=CARTESIAN_POINT('Ctrl Pts',(5.883324066422,1.04964479963234,-1.35191858333315));
#34193=CARTESIAN_POINT('Ctrl Pts',(6.02592910385855,1.68891108077235,-0.0198425009263074));
#34194=CARTESIAN_POINT('Ctrl Pts',(6.15477896868988,1.10345053670017,1.17755753597987));
#34195=CARTESIAN_POINT('Ctrl Pts',(6.27054089751149,0.0181739231631492,
1.55116490184665));
#34196=CARTESIAN_POINT('Ctrl Pts',(6.37374590914519,-0.944877441319298,
1.21343625499497));
#34197=CARTESIAN_POINT('Ctrl Pts',(6.47603956445423,-1.48313972011788,0.354292762592425));
#34198=CARTESIAN_POINT('Ctrl Pts',(6.57752721567845,-1.36903420817986,-0.643670764365519));
#34199=CARTESIAN_POINT('Ctrl Pts',(6.67824768359502,-0.663252374784276,
-1.34885741154892));
#34200=CARTESIAN_POINT('Ctrl Pts',(6.77839723147235,0.322508461880067,-1.45796924039956));
#34201=CARTESIAN_POINT('Ctrl Pts',(6.86124765395301,1.01625734071238,-1.02232645390806));
#34202=CARTESIAN_POINT('Ctrl Pts',(6.92756787351227,1.31944073792609,-0.468256814773046));
#34203=CARTESIAN_POINT('Ctrl Pts',(6.96040226429529,1.37148079685521,-0.165228975162103));
#34204=CARTESIAN_POINT('Ctrl Pts',(6.97707472275653,1.3717745235424,-0.00657861409212436));
#34205=CARTESIAN_POINT('Ctrl Pts',(0.00161515851542798,1.53044829317965,
0.0269321480552476));
#34206=CARTESIAN_POINT('Ctrl Pts',(0.0201220759100287,1.53012224794576,
0.20303869712926));
#34207=CARTESIAN_POINT('Ctrl Pts',(0.0568934829114929,1.47197746737321,
0.542427739520397));
#34208=CARTESIAN_POINT('Ctrl Pts',(0.131095753839526,1.13271443757942,1.16232575285471));
#34209=CARTESIAN_POINT('Ctrl Pts',(0.224621021627344,0.35091150368134,1.65551025424783));
#34210=CARTESIAN_POINT('Ctrl Pts',(0.338286873126993,-0.768313442313391,
1.53243149360112));
#34211=CARTESIAN_POINT('Ctrl Pts',(0.453361445182077,-1.57547718717538,
0.728139909528747));
#34212=CARTESIAN_POINT('Ctrl Pts',(0.569884598800981,-1.70710757953583,
-0.418100970988217));
#34213=CARTESIAN_POINT('Ctrl Pts',(0.687857467706789,-1.08784745868724,
-1.40832549057182));
#34214=CARTESIAN_POINT('Ctrl Pts',(0.807288840150634,0.0280726252692547,
-1.80167751441015));
#34215=CARTESIAN_POINT('Ctrl Pts',(0.914740219816513,1.03198965030329,-1.45112979405465));
#34216=CARTESIAN_POINT('Ctrl Pts',(1.00969670875881,1.59968282864761,-0.738184106724425));
#34217=CARTESIAN_POINT('Ctrl Pts',(1.09172273732053,1.77602714402117,0.0285405148911991));
#34218=CARTESIAN_POINT('Ctrl Pts',(1.17437872066553,1.59987524911727,0.801458775626711));
#34219=CARTESIAN_POINT('Ctrl Pts',(1.25765544748547,1.10238644594154,1.4275960011703));
#34220=CARTESIAN_POINT('Ctrl Pts',(1.34154470845672,0.378319431930998,1.7746505260415));
#34221=CARTESIAN_POINT('Ctrl Pts',(1.45419701031386,-0.705136228348483,
1.78339235323209));
#34222=CARTESIAN_POINT('Ctrl Pts',(1.59648741121626,-1.8563330628512,0.871461571340324));
#34223=CARTESIAN_POINT('Ctrl Pts',(1.74064586963647,-1.86249944592916,-0.621030337744628));
#34224=CARTESIAN_POINT('Ctrl Pts',(1.85702935773388,-1.15881384850636,-1.4902952011907));
#34225=CARTESIAN_POINT('Ctrl Pts',(1.97409322998411,-0.15066510931235,-1.98428777225483));
#34226=CARTESIAN_POINT('Ctrl Pts',(2.12163828274568,1.34022641380533,-1.65398375350995));
#34227=CARTESIAN_POINT('Ctrl Pts',(2.30048850270571,2.14467296000503,0.0187913828637551));
#34228=CARTESIAN_POINT('Ctrl Pts',(2.45086488774202,1.47323008289345,1.4163874062059));
#34229=CARTESIAN_POINT('Ctrl Pts',(2.57186497454107,0.420695575966319,1.91549206070169));
#34230=CARTESIAN_POINT('Ctrl Pts',(2.66293836951461,-0.450677600870363,
1.91750519917846));
#34231=CARTESIAN_POINT('Ctrl Pts',(2.7543083824095,-1.24144775215012,1.53674405551446));
#34232=CARTESIAN_POINT('Ctrl Pts',(2.845945416743,-1.78973088627105,0.849726749694565));
#34233=CARTESIAN_POINT('Ctrl Pts',(2.93782583740514,-1.98537059820214,-0.00933625461138338));
#34234=CARTESIAN_POINT('Ctrl Pts',(3.0452661736348,-1.75766233264543,-1.01511590115231));
#34235=CARTESIAN_POINT('Ctrl Pts',(3.16835592453166,-0.899160965219046,
-1.87833647594073));
#34236=CARTESIAN_POINT('Ctrl Pts',(3.30713426793985,0.468701930885861,-2.03267167226986));
#34237=CARTESIAN_POINT('Ctrl Pts',(3.44612725137011,1.63270311246182,-1.29975466142584));
#34238=CARTESIAN_POINT('Ctrl Pts',(3.58521702248767,2.08828439185582,0.000128743541493508));
#34239=CARTESIAN_POINT('Ctrl Pts',(3.72430585843795,1.63321566517972,1.30001690797893));
#34240=CARTESIAN_POINT('Ctrl Pts',(3.86328811026007,0.467872078525812,2.03198524404679));
#34241=CARTESIAN_POINT('Ctrl Pts',(4.00206055629492,-0.897638539459245,
1.87766260277105));
#34242=CARTESIAN_POINT('Ctrl Pts',(4.14052047602126,-1.86669284198261,0.907716764412239));
#34243=CARTESIAN_POINT('Ctrl Pts',(4.27856708575799,-2.0189887304933,-0.450770285803224));
#34244=CARTESIAN_POINT('Ctrl Pts',(4.41610166348544,-1.29362389666168,-1.60345254256816));
#34245=CARTESIAN_POINT('Ctrl Pts',(4.55302789008076,-0.0135058866939321,
-2.050212795458));
#34246=CARTESIAN_POINT('Ctrl Pts',(4.68925261674667,1.25922415346523,-1.60354209644131));
#34247=CARTESIAN_POINT('Ctrl Pts',(4.82468558038221,1.9712326392338,-0.467118840728988));
#34248=CARTESIAN_POINT('Ctrl Pts',(4.95924592020433,1.82182897712141,0.856515477717086));
#34249=CARTESIAN_POINT('Ctrl Pts',(5.09284396200303,0.884552093304522,1.79121367849672));
#34250=CARTESIAN_POINT('Ctrl Pts',(5.21068038662158,-0.275570397721873,
1.91923933957688));
#34251=CARTESIAN_POINT('Ctrl Pts',(5.31307309209999,-1.15755384723355,1.49002958567083));
#34252=CARTESIAN_POINT('Ctrl Pts',(5.42941292464469,-1.86054864392746,0.619529830873306));
#34253=CARTESIAN_POINT('Ctrl Pts',(5.57351539554265,-1.85877020130954,-0.868886341085341));
#34254=CARTESIAN_POINT('Ctrl Pts',(5.74418971119599,-0.472056341979532,
-1.96814250186018));
#34255=CARTESIAN_POINT('Ctrl Pts',(5.91250379993996,1.22319597970524,-1.5739132963462));
#34256=CARTESIAN_POINT('Ctrl Pts',(6.07836620391931,1.96669257276546,-0.0244705791669788));
#34257=CARTESIAN_POINT('Ctrl Pts',(6.22809494634827,1.28580890149433,1.36676280853955));
#34258=CARTESIAN_POINT('Ctrl Pts',(6.36234254672962,0.0270514125726567,
1.79951128756652));
#34259=CARTESIAN_POINT('Ctrl Pts',(6.48171218482806,-1.08665979377014,1.40829938442376));
#34260=CARTESIAN_POINT('Ctrl Pts',(6.59962381806671,-1.70640593150187,0.417640574653327));
#34261=CARTESIAN_POINT('Ctrl Pts',(6.71608583977231,-1.57451406593522,-0.727604326553729));
#34262=CARTESIAN_POINT('Ctrl Pts',(6.83109988901939,-0.767942536703866,
-1.53166897248179));
#34263=CARTESIAN_POINT('Ctrl Pts',(6.94470644964824,0.350764911141124,-1.65459943602436));
#34264=CARTESIAN_POINT('Ctrl Pts',(7.03818284450952,1.13212881810176,-1.16171427974159));
#34265=CARTESIAN_POINT('Ctrl Pts',(7.1123475034697,1.47122577126917,-0.542122479375375));
#34266=CARTESIAN_POINT('Ctrl Pts',(7.14909956085597,1.52933816287858,-0.202914044278201));
#34267=CARTESIAN_POINT('Ctrl Pts',(7.16759750918473,1.52966405009522,-0.0268928421120539));
#34268=CARTESIAN_POINT('Ctrl Pts',(0.191650118418653,1.37200316952796,0.00666815673193312));
#34269=CARTESIAN_POINT('Ctrl Pts',(0.208325719758175,1.37170938746674,0.165348424386552));
#34270=CARTESIAN_POINT('Ctrl Pts',(0.241166543218968,1.31965892482236,0.468436764487971));
#34271=CARTESIAN_POINT('Ctrl Pts',(0.307500414610168,1.01641958147785,1.0226151319287));
#34272=CARTESIAN_POINT('Ctrl Pts',(0.390369372912809,0.322487480659442,
1.45839154679416));
#34273=CARTESIAN_POINT('Ctrl Pts',(0.490545507503801,-0.663481834066145,
1.34918217829499));
#34274=CARTESIAN_POINT('Ctrl Pts',(0.591296831845559,-1.36962537389197,
0.643945208842946));
#34275=CARTESIAN_POINT('Ctrl Pts',(0.692819022950002,-1.4834868198206,-0.354693992611235));
#34276=CARTESIAN_POINT('Ctrl Pts',(0.79515128124215,-0.945721582226587,
-1.21334885843603));
#34277=CARTESIAN_POINT('Ctrl Pts',(0.898397805393483,0.019124050649053,
-1.55286223755737));
#34278=CARTESIAN_POINT('Ctrl Pts',(0.991048529453213,0.884620402844577,
-1.25029479050423));
#34279=CARTESIAN_POINT('Ctrl Pts',(1.07280457269834,1.37332023443167,-0.636418491153494));
#34280=CARTESIAN_POINT('Ctrl Pts',(1.14337435396381,1.52497778900527,0.0232193216955604));
#34281=CARTESIAN_POINT('Ctrl Pts',(1.21445487160599,1.37347475326106,0.687882348496639));
#34282=CARTESIAN_POINT('Ctrl Pts',(1.28606621168212,0.945692747518926,1.22628909211129));
#34283=CARTESIAN_POINT('Ctrl Pts',(1.35822394446807,0.322887605036237,1.52484062894975));
#34284=CARTESIAN_POINT('Ctrl Pts',(1.45518726216361,-0.609556983176929,
1.53241846122719));
#34285=CARTESIAN_POINT('Ctrl Pts',(1.57783368086597,-1.60225845024684,0.746967726957822));
#34286=CARTESIAN_POINT('Ctrl Pts',(1.70249589452176,-1.60863592636691,-0.543521601599762));
#34287=CARTESIAN_POINT('Ctrl Pts',(1.80347019036147,-0.998354974154592,
-1.29794080715334));
#34288=CARTESIAN_POINT('Ctrl Pts',(1.90528174786493,-0.12178238469645,-1.72773866254481));
#34289=CARTESIAN_POINT('Ctrl Pts',(2.03415464227018,1.18048402935804,-1.44105642428614));
#34290=CARTESIAN_POINT('Ctrl Pts',(2.19137194686348,1.89005998100612,0.0282102837295534));
#34291=CARTESIAN_POINT('Ctrl Pts',(2.32454795335086,1.29747855460094,1.26686334860849));
#34292=CARTESIAN_POINT('Ctrl Pts',(2.43238000253166,0.359684880651055,1.71226358790709));
#34293=CARTESIAN_POINT('Ctrl Pts',(2.51389508088681,-0.420163686752707,
1.71436684276211));
#34294=CARTESIAN_POINT('Ctrl Pts',(2.59604473430107,-1.13126882064223,1.37245282944764));
#34295=CARTESIAN_POINT('Ctrl Pts',(2.67882608336087,-1.62685859758749,0.752138485726358));
#34296=CARTESIAN_POINT('Ctrl Pts',(2.76222187864817,-1.80485064039527,-0.0274796911837139));
#34297=CARTESIAN_POINT('Ctrl Pts',(2.86022959910713,-1.59768976513308,-0.944989781542403));
#34298=CARTESIAN_POINT('Ctrl Pts',(2.97324187521099,-0.810607665017154,
-1.73843407949934));
#34299=CARTESIAN_POINT('Ctrl Pts',(3.1016972315778,0.455113169607269,-1.88310324228184));
#34300=CARTESIAN_POINT('Ctrl Pts',(3.23139431556386,1.5422393319403,-1.20073842659454));
#34301=CARTESIAN_POINT('Ctrl Pts',(3.3623017082119,1.97273947585015,0.0219070491777476));
#34302=CARTESIAN_POINT('Ctrl Pts',(3.49434572163654,1.54259771177146,1.25649542936377));
#34303=CARTESIAN_POINT('Ctrl Pts',(3.6274603391642,0.427609280977633,1.95918845230357));
#34304=CARTESIAN_POINT('Ctrl Pts',(3.76157159803446,-0.89215437286064,1.81208933337819));
#34305=CARTESIAN_POINT('Ctrl Pts',(3.89660124235199,-1.83859312657177,0.867715935336504));
#34306=CARTESIAN_POINT('Ctrl Pts',(4.03246592923656,-1.99055769088599,-0.468958872232718));
#34307=CARTESIAN_POINT('Ctrl Pts',(4.16907822980912,-1.27190965259628,-1.61495361257738));
#34308=CARTESIAN_POINT('Ctrl Pts',(4.30634680696854,0.0106137187745297,
-2.06480696177015));
#34309=CARTESIAN_POINT('Ctrl Pts',(4.44417666851365,1.29894786746045,-1.61491946025705));
#34310=CARTESIAN_POINT('Ctrl Pts',(4.58247097086598,2.02777293713842,-0.455689806908409));
#34311=CARTESIAN_POINT('Ctrl Pts',(4.72112199455802,1.87589664300924,0.908314574073854));
#34312=CARTESIAN_POINT('Ctrl Pts',(4.86004315540616,0.902897634535989,1.88170990575402));
#34313=CARTESIAN_POINT('Ctrl Pts',(4.98366759096385,-0.314015698055534,
2.01785190496137));
#34314=CARTESIAN_POINT('Ctrl Pts',(5.09187133849345,-1.24637851798351,1.56480044764036));
#34315=CARTESIAN_POINT('Ctrl Pts',(5.21552467151859,-1.99407016576495,0.640432896817704));
#34316=CARTESIAN_POINT('Ctrl Pts',(5.3699969526124,-1.99604585088204,-0.954985827792077));
#34317=CARTESIAN_POINT('Ctrl Pts',(5.55496725528798,-0.496223154682238,
-2.14999595683691));
#34318=CARTESIAN_POINT('Ctrl Pts',(5.73929698552342,1.36136728950175,-1.7225381487768));
#34319=CARTESIAN_POINT('Ctrl Pts',(5.92275132000792,2.18746307299438,-0.0106556007638544));
#34320=CARTESIAN_POINT('Ctrl Pts',(6.08990782660862,1.43044508811081,1.5441079994423));
#34321=CARTESIAN_POINT('Ctrl Pts',(6.24090189886119,0.0150536285141992,
2.03247023467283));
#34322=CARTESIAN_POINT('Ctrl Pts',(6.37596384346278,-1.245467488101,1.59099367856498));
#34323=CARTESIAN_POINT('Ctrl Pts',(6.51011494443758,-1.95157823607613,0.464639836930734));
#34324=CARTESIAN_POINT('Ctrl Pts',(6.64326231244002,-1.80182018279085,-0.844992615596695));
#34325=CARTESIAN_POINT('Ctrl Pts',(6.77536637951215,-0.876213641136945,
-1.76877236414733));
#34326=CARTESIAN_POINT('Ctrl Pts',(6.90628636007342,0.413337672718451,-1.91167105187073));
#34327=CARTESIAN_POINT('Ctrl Pts',(7.01449296705847,1.317278997971,-1.34103733354681));
#34328=CARTESIAN_POINT('Ctrl Pts',(7.10025971255133,1.70991664822488,-0.624645108920693));
#34329=CARTESIAN_POINT('Ctrl Pts',(7.14305493470294,1.77751904014347,-0.229658083660462));
#34330=CARTESIAN_POINT('Ctrl Pts',(7.16435095364275,1.77789422231039,-0.0270112393448257));
#34331=CARTESIAN_POINT('Ctrl Pts',(0.433579734615651,1.42338264829905,-0.0186609375666422));
#34332=CARTESIAN_POINT('Ctrl Pts',(0.45077175068432,1.42307976831204,0.144933385405884));
#34333=CARTESIAN_POINT('Ctrl Pts',(0.484766255202398,1.36910205511848,0.458630441946588));
#34334=CARTESIAN_POINT('Ctrl Pts',(0.552904217423861,1.05717509657061,1.02775607980824));
#34335=CARTESIAN_POINT('Ctrl Pts',(0.637261343794741,0.349940230409029,
1.46993737614911));
#34336=CARTESIAN_POINT('Ctrl Pts',(0.737955078347263,-0.64090291216559,
1.35804969385912));
#34337=CARTESIAN_POINT('Ctrl Pts',(0.837958305020876,-1.34029379299783,
0.656595041185004));
#34338=CARTESIAN_POINT('Ctrl Pts',(0.937469751658734,-1.44986143925427,
-0.322474352691997));
#34339=CARTESIAN_POINT('Ctrl Pts',(1.03653768857201,-0.927532143269398,
-1.15270388821428));
#34340=CARTESIAN_POINT('Ctrl Pts',(1.13528664206825,-0.00406063929822328,
-1.47553624283577));
#34341=CARTESIAN_POINT('Ctrl Pts',(1.22285503142353,0.813435828702286,-1.18804460975032));
#34342=CARTESIAN_POINT('Ctrl Pts',(1.2994077250104,1.27049736626634,-0.612887311395251));
#34343=CARTESIAN_POINT('Ctrl Pts',(1.36499674892347,1.41100310001544,0.00035353166708084));
#34344=CARTESIAN_POINT('Ctrl Pts',(1.43059568312704,1.27070020510333,0.61366388234097));
#34345=CARTESIAN_POINT('Ctrl Pts',(1.4962312545865,0.878209084856175,1.10687935212739));
#34346=CARTESIAN_POINT('Ctrl Pts',(1.56193801594905,0.310932069106502,1.37839912120734));
#34347=CARTESIAN_POINT('Ctrl Pts',(1.64967414989946,-0.53309404837248,1.38454132805412));
#34348=CARTESIAN_POINT('Ctrl Pts',(1.75967689190248,-1.42179124988727,0.677917697927037));
#34349=CARTESIAN_POINT('Ctrl Pts',(1.87030374837707,-1.42492338598861,-0.467528578572644));
#34350=CARTESIAN_POINT('Ctrl Pts',(1.95930615128506,-0.886719411403927,
-1.13212549488085));
#34351=CARTESIAN_POINT('Ctrl Pts',(2.04868501593063,-0.116842483376934,
-1.50916256492749));
#34352=CARTESIAN_POINT('Ctrl Pts',(2.16113597918497,1.01949045845296,-1.25718641848022));
#34353=CARTESIAN_POINT('Ctrl Pts',(2.29753653972427,1.63359955754855,0.0182741116564148));
#34354=CARTESIAN_POINT('Ctrl Pts',(2.41255997285096,1.12092326938844,1.08784129807883));
#34355=CARTESIAN_POINT('Ctrl Pts',(2.50548250553227,0.312692840718015,1.47156942514894));
#34356=CARTESIAN_POINT('Ctrl Pts',(2.5756478252876,-0.358700517462746,1.47334788294029));
#34357=CARTESIAN_POINT('Ctrl Pts',(2.64631010793517,-0.970420591352287,
1.17915861370463));
#34358=CARTESIAN_POINT('Ctrl Pts',(2.71748033839573,-1.39658058337222,0.645750906017974));
#34359=CARTESIAN_POINT('Ctrl Pts',(2.78919511691523,-1.54965148821638,-0.0247331123591614));
#34360=CARTESIAN_POINT('Ctrl Pts',(2.87350305966914,-1.3714855406497,-0.814073759711593));
#34361=CARTESIAN_POINT('Ctrl Pts',(2.97078939013895,-0.693974426765108,
-1.4973274317204));
#34362=CARTESIAN_POINT('Ctrl Pts',(3.08153687990464,0.39749474778564,-1.62249875077181));
#34363=CARTESIAN_POINT('Ctrl Pts',(3.1936745402062,1.33779004137835,-1.03288036662484));
#34364=CARTESIAN_POINT('Ctrl Pts',(3.30718845046989,1.71177951199544,0.0272883049770704));
#34365=CARTESIAN_POINT('Ctrl Pts',(3.42212730901466,1.33803574566457,1.10238120232907));
#34366=CARTESIAN_POINT('Ctrl Pts',(3.538506378401,0.363549106704547,1.71759100272943));
#34367=CARTESIAN_POINT('Ctrl Pts',(3.65633855270862,-0.796304462599152,
1.58934728787291));
#34368=CARTESIAN_POINT('Ctrl Pts',(3.77562775390538,-1.63334363828854,0.755741510627042));
#34369=CARTESIAN_POINT('Ctrl Pts',(3.89637125571665,-1.76965210710189,-0.432192879453737));
#34370=CARTESIAN_POINT('Ctrl Pts',(4.01855873411348,-1.12794076480263,-1.45803741696457));
#34371=CARTESIAN_POINT('Ctrl Pts',(4.14217229917805,0.0266723610995444,
-1.86455751754551));
#34372=CARTESIAN_POINT('Ctrl Pts',(4.26718715875757,1.19587440059458,-1.45789650543289));
#34373=CARTESIAN_POINT('Ctrl Pts',(4.39356916365005,1.86336783373069,-0.399233077619641));
#34374=CARTESIAN_POINT('Ctrl Pts',(4.5212929060358,1.72515502607219,0.857488857248103));
#34375=CARTESIAN_POINT('Ctrl Pts',(4.65028582120944,0.822837389786965,1.76269613439977));
#34376=CARTESIAN_POINT('Ctrl Pts',(4.76604443107118,-0.316629397701036,
1.89185367539892));
#34377=CARTESIAN_POINT('Ctrl Pts',(4.86809768231334,-1.1964095449954,1.46496928641178));
#34378=CARTESIAN_POINT('Ctrl Pts',(4.98539825189974,-1.90620592827337,0.588811917862644));
#34379=CARTESIAN_POINT('Ctrl Pts',(5.1332295071313,-1.91202735868246,-0.938044171791657));
#34380=CARTESIAN_POINT('Ctrl Pts',(5.31238298578506,-0.462560121218143,
-2.09951488460516));
#34381=CARTESIAN_POINT('Ctrl Pts',(5.49310436300435,1.35991583640525,-1.68538171905435));
#34382=CARTESIAN_POINT('Ctrl Pts',(5.67518902663768,2.18456796062644,0.0113588410607889));
#34383=CARTESIAN_POINT('Ctrl Pts',(5.84314793625201,1.42809693145233,1.57583744405794));
#34384=CARTESIAN_POINT('Ctrl Pts',(5.99651346043047,-0.00890518390018798,
2.07429703179719));
#34385=CARTESIAN_POINT('Ctrl Pts',(6.13495786102797,-1.30163918905444,1.6236443878012));
#34386=CARTESIAN_POINT('Ctrl Pts',(6.27372909181613,-2.03382659165114,0.459724741300774));
#34387=CARTESIAN_POINT('Ctrl Pts',(6.41269993312306,-1.87954606508905,-0.907477856997402));
#34388=CARTESIAN_POINT('Ctrl Pts',(6.55182430461631,-0.906300332924981,
-1.88153117457102));
#34389=CARTESIAN_POINT('Ctrl Pts',(6.69087755354555,0.463291981836397,-2.03547998152785));
#34390=CARTESIAN_POINT('Ctrl Pts',(6.8068530207987,1.43257691496249,-1.42501755139953));
#34391=CARTESIAN_POINT('Ctrl Pts',(6.89923554548022,1.85603723916337,-0.653520444359812));
#34392=CARTESIAN_POINT('Ctrl Pts',(6.94565012946822,1.92942310320324,-0.225166386510263));
#34393=CARTESIAN_POINT('Ctrl Pts',(6.96860631615056,1.92982753334055,-0.00672185930328364));
#34394=CARTESIAN_POINT('Ctrl Pts',(0.507274282535025,1.57083221824462,-0.0261324580079617));
#34395=CARTESIAN_POINT('Ctrl Pts',(0.526112754645697,1.57050033185239,0.153129071208421));
#34396=CARTESIAN_POINT('Ctrl Pts',(0.563671099889176,1.51089822523919,0.499712748256306));
#34397=CARTESIAN_POINT('Ctrl Pts',(0.638531587307084,1.16784235604667,1.12489642057377));
#34398=CARTESIAN_POINT('Ctrl Pts',(0.731169346030264,0.391386187333621,
1.61031900017172));
#34399=CARTESIAN_POINT('Ctrl Pts',(0.841237656753425,-0.691876171660509,
1.48695593269843));
#34400=CARTESIAN_POINT('Ctrl Pts',(0.950117270175318,-1.45259978153303,
0.722851743027934));
#34401=CARTESIAN_POINT('Ctrl Pts',(1.05791430831992,-1.57031827941192,-0.337921120658705));
#34402=CARTESIAN_POINT('Ctrl Pts',(1.16466136624435,-1.00664473279018,-1.23180991269817));
#34403=CARTESIAN_POINT('Ctrl Pts',(1.27042439012675,-0.0172220148914788,
-1.5764787034829));
#34404=CARTESIAN_POINT('Ctrl Pts',(1.36363143937566,0.852328804108645,-1.26948855586366));
#34405=CARTESIAN_POINT('Ctrl Pts',(1.44462089157926,1.33552310991331,-0.660772156033481));
#34406=CARTESIAN_POINT('Ctrl Pts',(1.51369502886818,1.48307233184017,-0.0149411033225211));
#34407=CARTESIAN_POINT('Ctrl Pts',(1.58243335031582,1.33571785928905,0.627597621853533));
#34408=CARTESIAN_POINT('Ctrl Pts',(1.65086776854819,0.926180438835773,1.14147824220308));
#34409=CARTESIAN_POINT('Ctrl Pts',(1.71901564079579,0.337798744691098,1.42277664606786));
#34410=CARTESIAN_POINT('Ctrl Pts',(1.80954699166651,-0.533138243710397,
1.42838884196275));
#34411=CARTESIAN_POINT('Ctrl Pts',(1.92211699882143,-1.44076854634821,0.703312487395003));
#34412=CARTESIAN_POINT('Ctrl Pts',(2.03410697282657,-1.44096567761035,-0.45603039345914));
#34413=CARTESIAN_POINT('Ctrl Pts',(2.12343975147708,-0.900622955850315,
-1.1223056389964));
#34414=CARTESIAN_POINT('Ctrl Pts',(2.21262722357295,-0.132081188978774,
-1.49810670491376));
#34415=CARTESIAN_POINT('Ctrl Pts',(2.32400115347409,0.99212176527143,-1.24571725700378));
#34416=CARTESIAN_POINT('Ctrl Pts',(2.45753819177609,1.58991663374091,0.00400964696824968));
#34417=CARTESIAN_POINT('Ctrl Pts',(2.56896324607187,1.0911031110618,1.03867404971372));
#34418=CARTESIAN_POINT('Ctrl Pts',(2.65830689011116,0.314148482822285,1.40686816583826));
#34419=CARTESIAN_POINT('Ctrl Pts',(2.72544249781257,-0.328068046776882,
1.40825091301288));
#34420=CARTESIAN_POINT('Ctrl Pts',(2.79272924072257,-0.910251615434656,
1.12786562955998));
#34421=CARTESIAN_POINT('Ctrl Pts',(2.86020818788873,-1.31386839710613,0.622124005734457));
#34422=CARTESIAN_POINT('Ctrl Pts',(2.92787301289815,-1.45800869363228,-0.0104270331006981));
#34423=CARTESIAN_POINT('Ctrl Pts',(3.00708815442165,-1.29025655858587,-0.751868478198773));
#34424=CARTESIAN_POINT('Ctrl Pts',(3.09806652405742,-0.656258052591304,
-1.39010016384697));
#34425=CARTESIAN_POINT('Ctrl Pts',(3.20112002170027,0.358888315027333,-1.50555498910911));
#34426=CARTESIAN_POINT('Ctrl Pts',(3.30486699671298,1.22824795529413,-0.959553219448269));
#34427=CARTESIAN_POINT('Ctrl Pts',(3.40947097081598,1.57205004825354,0.0172505142157691));
#34428=CARTESIAN_POINT('Ctrl Pts',(3.51496482062722,1.22855626968513,1.00343097025568));
#34429=CARTESIAN_POINT('Ctrl Pts',(3.62142414278527,0.337170590068482,1.56556264385462));
#34430=CARTESIAN_POINT('Ctrl Pts',(3.7289101906844,-0.72044261482484,1.44818418374162));
#34431=CARTESIAN_POINT('Ctrl Pts',(3.83748189048483,-1.48179526817998,0.689478939216293));
#34432=CARTESIAN_POINT('Ctrl Pts',(3.94719105937069,-1.60536811159166,-0.389593160174116));
#34433=CARTESIAN_POINT('Ctrl Pts',(4.05808411613347,-1.02302204204489,-1.3202678117195));
#34434=CARTESIAN_POINT('Ctrl Pts',(4.17020177333295,0.023945317461627,-1.68883397376188));
#34435=CARTESIAN_POINT('Ctrl Pts',(4.28357766789648,1.08402787750074,-1.32017808730271));
#34436=CARTESIAN_POINT('Ctrl Pts',(4.39824273901555,1.68964083833592,-0.360000126936474));
#34437=CARTESIAN_POINT('Ctrl Pts',(4.51419461860112,1.56435375572891,0.780776691995831));
#34438=CARTESIAN_POINT('Ctrl Pts',(4.63149231723297,0.744360778919685,1.60396130772566));
#34439=CARTESIAN_POINT('Ctrl Pts',(4.73693160879815,-0.293325697447064,
1.72194634915242));
#34440=CARTESIAN_POINT('Ctrl Pts',(4.83004564060015,-1.09603579295444,1.3326447194401));
#34441=CARTESIAN_POINT('Ctrl Pts',(4.93724867578556,-1.74478074698819,0.532228279741075));
#34442=CARTESIAN_POINT('Ctrl Pts',(5.0727192263256,-1.75135757443499,-0.866786972823142));
#34443=CARTESIAN_POINT('Ctrl Pts',(5.2375920787962,-0.418735016597171,-1.93699754149329));
#34444=CARTESIAN_POINT('Ctrl Pts',(5.40471142470201,1.26692786505107,-1.55606606404468));
#34445=CARTESIAN_POINT('Ctrl Pts',(5.57399875094415,2.03565424341948,0.0202999121532512));
#34446=CARTESIAN_POINT('Ctrl Pts',(5.73107580726873,1.33028224859866,1.48442877087329));
#34447=CARTESIAN_POINT('Ctrl Pts',(5.87529457722589,-0.0207131719272176,
1.95442357858293));
#34448=CARTESIAN_POINT('Ctrl Pts',(6.0061289456163,-1.24277852622533,1.52958044066593));
#34449=CARTESIAN_POINT('Ctrl Pts',(6.1379456646946,-1.93936778890619,0.424561021508401));
#34450=CARTESIAN_POINT('Ctrl Pts',(6.27066300628487,-1.79326538900601,-0.881319784202494));
#34451=CARTESIAN_POINT('Ctrl Pts',(6.40424425838086,-0.859607066663113,
-1.81773053787805));
#34452=CARTESIAN_POINT('Ctrl Pts',(6.53853932211068,0.462976199094479,-1.96763098468602));
#34453=CARTESIAN_POINT('Ctrl Pts',(6.65112996586297,1.404881072604,-1.37595823609957));
#34454=CARTESIAN_POINT('Ctrl Pts',(6.74131168525227,1.81841870776265,-0.622862303654825));
#34455=CARTESIAN_POINT('Ctrl Pts',(6.78671559508214,1.89026514761845,-0.203833176009383));
#34456=CARTESIAN_POINT('Ctrl Pts',(6.80919797775352,1.89066123052353,0.0101027673201533));
#34457=CARTESIAN_POINT('Ctrl Pts',(0.508591862447781,1.64562043801211,-0.0261324580079617));
#34458=CARTESIAN_POINT('Ctrl Pts',(0.528271024599208,1.6452737407805,0.161128837931408));
#34459=CARTESIAN_POINT('Ctrl Pts',(0.567647573513685,1.58281094560678,0.524492831752905));
#34460=CARTESIAN_POINT('Ctrl Pts',(0.645996560435206,1.22365592193525,1.1787804941138));
#34461=CARTESIAN_POINT('Ctrl Pts',(0.743073641882897,0.410281924307437,
1.68766009875447));
#34462=CARTESIAN_POINT('Ctrl Pts',(0.858352417401347,-0.724396860085975,
1.55831173688398));
#34463=CARTESIAN_POINT('Ctrl Pts',(0.972375295448021,-1.52098532662473,
0.758217612597792));
#34464=CARTESIAN_POINT('Ctrl Pts',(1.08519171777668,-1.64409811634449,-0.352032188510366));
#34465=CARTESIAN_POINT('Ctrl Pts',(1.19681996654867,-1.05450947578872,-1.28675893283186));
#34466=CARTESIAN_POINT('Ctrl Pts',(1.30730161177351,-0.0208333311052113,
-1.64663068201152));
#34467=CARTESIAN_POINT('Ctrl Pts',(1.40452364629174,0.886236470079679,-1.32621345051066));
#34468=CARTESIAN_POINT('Ctrl Pts',(1.48890750188156,1.38959463750653,-0.691912415510853));
#34469=CARTESIAN_POINT('Ctrl Pts',(1.56078188611823,1.54308896603543,-0.0198177610475133));
#34470=CARTESIAN_POINT('Ctrl Pts',(1.63221817171176,1.38983552550406,0.647948130516392));
#34471=CARTESIAN_POINT('Ctrl Pts',(1.70323404319384,0.964738946565908,1.1812205675546));
#34472=CARTESIAN_POINT('Ctrl Pts',(1.77384798276294,0.354991450441324,1.47260961294232));
#34473=CARTESIAN_POINT('Ctrl Pts',(1.86748993119896,-0.546099502039117,
1.47825694934893));
#34474=CARTESIAN_POINT('Ctrl Pts',(1.98363667823136,-1.48203264186415,0.7293081873873));
#34475=CARTESIAN_POINT('Ctrl Pts',(2.09871900316068,-1.48120258062414,-0.462340692211473));
#34476=CARTESIAN_POINT('Ctrl Pts',(2.19023826573612,-0.927379733426102,
-1.14481302651884));
#34477=CARTESIAN_POINT('Ctrl Pts',(2.2814255547235,-0.141378759287938,-1.52891931607764));
#34478=CARTESIAN_POINT('Ctrl Pts',(2.39484749559815,1.00382275253285,-1.27061478852019));
#34479=CARTESIAN_POINT('Ctrl Pts',(2.53025681997088,1.60865186335246,-0.00254459019504153));
#34480=CARTESIAN_POINT('Ctrl Pts',(2.64269039045238,1.10418776314993,1.04117197496908));
#34481=CARTESIAN_POINT('Ctrl Pts',(2.73249952801582,0.322974585676589,1.41105820876749));
#34482=CARTESIAN_POINT('Ctrl Pts',(2.7998141074244,-0.32110895921182,1.41232437949226));
#34483=CARTESIAN_POINT('Ctrl Pts',(2.86711382621074,-0.903428721470414,
1.13164638734841));
#34484=CARTESIAN_POINT('Ctrl Pts',(2.93442516377676,-1.30601623783849,0.626923391067463));
#34485=CARTESIAN_POINT('Ctrl Pts',(3.00177556402078,-1.44931171614156,-0.00280700337714968));
#34486=CARTESIAN_POINT('Ctrl Pts',(3.08042754178598,-1.28252605621248,-0.73905091180395));
#34487=CARTESIAN_POINT('Ctrl Pts',(3.17046965462109,-0.654511755766728,
-1.3704712298758));
#34488=CARTESIAN_POINT('Ctrl Pts',(3.27206448378161,0.346719679199525,-1.483704431146));
#34489=CARTESIAN_POINT('Ctrl Pts',(3.3740442463093,1.20102786916375,-0.946430056825302));
#34490=CARTESIAN_POINT('Ctrl Pts',(3.47649477143674,1.53732148053407,0.0107120740773195));
#34491=CARTESIAN_POINT('Ctrl Pts',(3.57949954098879,1.20134163447082,0.973667458417707));
#34492=CARTESIAN_POINT('Ctrl Pts',(3.68313928551533,0.333095090941954,1.52059902024328));
#34493=CARTESIAN_POINT('Ctrl Pts',(3.78749120379714,-0.693842597912142,
1.40614340263662));
#34494=CARTESIAN_POINT('Ctrl Pts',(3.89262893585172,-1.43094857905026,0.670971912346831));
#34495=CARTESIAN_POINT('Ctrl Pts',(3.99862203011025,-1.5499543985351,-0.371794281933162));
#34496=CARTESIAN_POINT('Ctrl Pts',(4.10553567293418,-0.988090997030439,
-1.26903707993744));
#34497=CARTESIAN_POINT('Ctrl Pts',(4.21343045112327,0.0197202801860453,
-1.62347464599002));
#34498=CARTESIAN_POINT('Ctrl Pts',(4.32236196180067,1.03832038776908,-1.26894288895586));
#34499=CARTESIAN_POINT('Ctrl Pts',(4.43238051112357,1.61925828890368,-0.34739423883176));
#34500=CARTESIAN_POINT('Ctrl Pts',(4.54353062752128,1.4989897755625,0.74620181404568));
#34501=CARTESIAN_POINT('Ctrl Pts',(4.65585125526312,0.71351870218781,1.53444845290457));
#34502=CARTESIAN_POINT('Ctrl Pts',(4.75676135685292,-0.279697500338493,
1.64729603227415));
#34503=CARTESIAN_POINT('Ctrl Pts',(4.84585493867587,-1.04780204615629,1.27474307821934));
#34504=CARTESIAN_POINT('Ctrl Pts',(4.94841313843452,-1.66845031883017,0.508931034591464));
#34505=CARTESIAN_POINT('Ctrl Pts',(5.07800659502253,-1.67475443904525,-0.829467776745351));
#34506=CARTESIAN_POINT('Ctrl Pts',(5.23577771702336,-0.399579932550961,
-1.85373353020478));
#34507=CARTESIAN_POINT('Ctrl Pts',(5.39581269472486,1.21472097060722,-1.48922395511139));
#34508=CARTESIAN_POINT('Ctrl Pts',(5.55809610080897,1.95203227446324,0.0217272724024816));
#34509=CARTESIAN_POINT('Ctrl Pts',(5.70888367040444,1.27533356599845,1.42745494534175));
#34510=CARTESIAN_POINT('Ctrl Pts',(5.84753617842438,-0.0234051752573978,
1.87960329280061));
#34511=CARTESIAN_POINT('Ctrl Pts',(5.9735033792588,-1.2000636353636,1.47084402209574));
#34512=CARTESIAN_POINT('Ctrl Pts',(6.10061934653175,-1.87205652425054,0.4054527917675));
#34513=CARTESIAN_POINT('Ctrl Pts',(6.22882892874595,-1.73128184695155,-0.856020464879398));
#34514=CARTESIAN_POINT('Ctrl Pts',(6.35811249074499,-0.82796691613823,-1.76256406416465));
#34515=CARTESIAN_POINT('Ctrl Pts',(6.48835538046169,0.454518312141212,-1.90827828922266));
#34516=CARTESIAN_POINT('Ctrl Pts',(6.59776527270895,1.37009311469038,-1.33377327146165));
#34517=CARTESIAN_POINT('Ctrl Pts',(6.68557306476182,1.77276616876359,-0.600525447669764));
#34518=CARTESIAN_POINT('Ctrl Pts',(6.72979494253028,1.84279755540219,-0.192431284750887));
#34519=CARTESIAN_POINT('Ctrl Pts',(6.75172308477496,1.84318387398818,0.016230664703078));
#34520=CARTESIAN_POINT('',(0.508591862447781,1.64562043801211,-0.0261324580079617));
#34521=CARTESIAN_POINT('Origin',(0.26,1.65,1.37288700589905E-18));
#34522=CARTESIAN_POINT('',(6.75172308477496,1.84318387398818,0.016230664703078));
#34523=CARTESIAN_POINT('Ctrl Pts',(0.508591862447781,1.64562043801211,-0.0261324580079617));
#34524=CARTESIAN_POINT('Ctrl Pts',(0.528271024599208,1.6452737407805,0.161128837931408));
#34525=CARTESIAN_POINT('Ctrl Pts',(0.567647573513685,1.58281094560678,0.524492831752905));
#34526=CARTESIAN_POINT('Ctrl Pts',(0.645996560435206,1.22365592193525,1.1787804941138));
#34527=CARTESIAN_POINT('Ctrl Pts',(0.743073641882897,0.410281924307437,
1.68766009875447));
#34528=CARTESIAN_POINT('Ctrl Pts',(0.858352417401347,-0.724396860085975,
1.55831173688398));
#34529=CARTESIAN_POINT('Ctrl Pts',(0.972375295448021,-1.52098532662473,
0.758217612597792));
#34530=CARTESIAN_POINT('Ctrl Pts',(1.08519171777668,-1.64409811634449,-0.352032188510366));
#34531=CARTESIAN_POINT('Ctrl Pts',(1.19681996654867,-1.05450947578872,-1.28675893283186));
#34532=CARTESIAN_POINT('Ctrl Pts',(1.30730161177351,-0.0208333311052113,
-1.64663068201152));
#34533=CARTESIAN_POINT('Ctrl Pts',(1.40452364629174,0.886236470079679,-1.32621345051066));
#34534=CARTESIAN_POINT('Ctrl Pts',(1.48890750188156,1.38959463750653,-0.691912415510853));
#34535=CARTESIAN_POINT('Ctrl Pts',(1.56078188611823,1.54308896603543,-0.0198177610475133));
#34536=CARTESIAN_POINT('Ctrl Pts',(1.63221817171176,1.38983552550406,0.647948130516392));
#34537=CARTESIAN_POINT('Ctrl Pts',(1.70323404319384,0.964738946565908,1.1812205675546));
#34538=CARTESIAN_POINT('Ctrl Pts',(1.77384798276294,0.354991450441324,1.47260961294232));
#34539=CARTESIAN_POINT('Ctrl Pts',(1.86748993119896,-0.546099502039117,
1.47825694934893));
#34540=CARTESIAN_POINT('Ctrl Pts',(1.98363667823136,-1.48203264186415,0.7293081873873));
#34541=CARTESIAN_POINT('Ctrl Pts',(2.09871900316068,-1.48120258062414,-0.462340692211473));
#34542=CARTESIAN_POINT('Ctrl Pts',(2.19023826573612,-0.927379733426102,
-1.14481302651884));
#34543=CARTESIAN_POINT('Ctrl Pts',(2.2814255547235,-0.141378759287938,-1.52891931607764));
#34544=CARTESIAN_POINT('Ctrl Pts',(2.39484749559815,1.00382275253285,-1.27061478852019));
#34545=CARTESIAN_POINT('Ctrl Pts',(2.53025681997088,1.60865186335246,-0.00254459019504153));
#34546=CARTESIAN_POINT('Ctrl Pts',(2.64269039045238,1.10418776314993,1.04117197496908));
#34547=CARTESIAN_POINT('Ctrl Pts',(2.73249952801582,0.322974585676589,1.41105820876749));
#34548=CARTESIAN_POINT('Ctrl Pts',(2.7998141074244,-0.32110895921182,1.41232437949226));
#34549=CARTESIAN_POINT('Ctrl Pts',(2.86711382621074,-0.903428721470414,
1.13164638734841));
#34550=CARTESIAN_POINT('Ctrl Pts',(2.93442516377676,-1.30601623783849,0.626923391067463));
#34551=CARTESIAN_POINT('Ctrl Pts',(3.00177556402078,-1.44931171614156,-0.00280700337714968));
#34552=CARTESIAN_POINT('Ctrl Pts',(3.08042754178598,-1.28252605621248,-0.73905091180395));
#34553=CARTESIAN_POINT('Ctrl Pts',(3.17046965462109,-0.654511755766728,
-1.3704712298758));
#34554=CARTESIAN_POINT('Ctrl Pts',(3.27206448378161,0.346719679199525,-1.483704431146));
#34555=CARTESIAN_POINT('Ctrl Pts',(3.3740442463093,1.20102786916375,-0.946430056825302));
#34556=CARTESIAN_POINT('Ctrl Pts',(3.47649477143674,1.53732148053407,0.0107120740773195));
#34557=CARTESIAN_POINT('Ctrl Pts',(3.57949954098879,1.20134163447082,0.973667458417707));
#34558=CARTESIAN_POINT('Ctrl Pts',(3.68313928551533,0.333095090941954,1.52059902024328));
#34559=CARTESIAN_POINT('Ctrl Pts',(3.78749120379714,-0.693842597912142,
1.40614340263662));
#34560=CARTESIAN_POINT('Ctrl Pts',(3.89262893585172,-1.43094857905026,0.670971912346831));
#34561=CARTESIAN_POINT('Ctrl Pts',(3.99862203011025,-1.5499543985351,-0.371794281933162));
#34562=CARTESIAN_POINT('Ctrl Pts',(4.10553567293418,-0.988090997030439,
-1.26903707993744));
#34563=CARTESIAN_POINT('Ctrl Pts',(4.21343045112327,0.0197202801860453,
-1.62347464599002));
#34564=CARTESIAN_POINT('Ctrl Pts',(4.32236196180067,1.03832038776908,-1.26894288895586));
#34565=CARTESIAN_POINT('Ctrl Pts',(4.43238051112357,1.61925828890368,-0.34739423883176));
#34566=CARTESIAN_POINT('Ctrl Pts',(4.54353062752128,1.4989897755625,0.74620181404568));
#34567=CARTESIAN_POINT('Ctrl Pts',(4.65585125526312,0.71351870218781,1.53444845290457));
#34568=CARTESIAN_POINT('Ctrl Pts',(4.75676135685292,-0.279697500338493,
1.64729603227415));
#34569=CARTESIAN_POINT('Ctrl Pts',(4.84585493867587,-1.04780204615629,1.27474307821934));
#34570=CARTESIAN_POINT('Ctrl Pts',(4.94841313843452,-1.66845031883017,0.508931034591464));
#34571=CARTESIAN_POINT('Ctrl Pts',(5.07800659502253,-1.67475443904525,-0.829467776745351));
#34572=CARTESIAN_POINT('Ctrl Pts',(5.23577771702336,-0.399579932550961,
-1.85373353020478));
#34573=CARTESIAN_POINT('Ctrl Pts',(5.39581269472486,1.21472097060722,-1.48922395511139));
#34574=CARTESIAN_POINT('Ctrl Pts',(5.55809610080897,1.95203227446324,0.0217272724024816));
#34575=CARTESIAN_POINT('Ctrl Pts',(5.70888367040444,1.27533356599845,1.42745494534175));
#34576=CARTESIAN_POINT('Ctrl Pts',(5.84753617842438,-0.0234051752573978,
1.87960329280061));
#34577=CARTESIAN_POINT('Ctrl Pts',(5.9735033792588,-1.2000636353636,1.47084402209574));
#34578=CARTESIAN_POINT('Ctrl Pts',(6.10061934653175,-1.87205652425054,0.4054527917675));
#34579=CARTESIAN_POINT('Ctrl Pts',(6.22882892874595,-1.73128184695155,-0.856020464879398));
#34580=CARTESIAN_POINT('Ctrl Pts',(6.35811249074499,-0.82796691613823,-1.76256406416465));
#34581=CARTESIAN_POINT('Ctrl Pts',(6.48835538046169,0.454518312141212,-1.90827828922266));
#34582=CARTESIAN_POINT('Ctrl Pts',(6.59776527270895,1.37009311469038,-1.33377327146165));
#34583=CARTESIAN_POINT('Ctrl Pts',(6.68557306476182,1.77276616876359,-0.600525447669764));
#34584=CARTESIAN_POINT('Ctrl Pts',(6.72979494253028,1.84279755540219,-0.192431284750887));
#34585=CARTESIAN_POINT('Ctrl Pts',(6.75172308477496,1.84318387398818,0.016230664703078));
#34586=CARTESIAN_POINT('Origin',(6.90957287525381,1.65,-2.42861286636753E-15));
#34587=CARTESIAN_POINT('Origin',(6.90957287525381,1.65,-2.42861286636753E-15));
#34588=CARTESIAN_POINT('Origin',(0.26,1.65,1.37288700589905E-18));
#34589=CARTESIAN_POINT('',(0.,0.,0.));
#34590=CARTESIAN_POINT('Origin',(2.1,0.,0.));
#34591=CARTESIAN_POINT('',(0.708327496212055,-2.45360913320878,0.00150472093799672));
#34592=CARTESIAN_POINT('',(0.592672503787945,-2.45282685237657,0.00258448634202159));
#34593=CARTESIAN_POINT('',(2.1,-2.4505,-3.00099698131059E-16));
#34594=CARTESIAN_POINT('',(0.4505,1.0763748274605,2.20373264345719));
#34595=CARTESIAN_POINT('Ctrl Pts',(0.708327496212055,-2.45360913320878,
0.00150472093799672));
#34596=CARTESIAN_POINT('Ctrl Pts',(0.704300982660464,-2.45411842762872,
0.0787150024977833));
#34597=CARTESIAN_POINT('Ctrl Pts',(0.700274469108872,-2.45079204224263,
0.15587784967814));
#34598=CARTESIAN_POINT('Ctrl Pts',(0.696247955557281,-2.44348687984151,
0.232658460786329));
#34599=CARTESIAN_POINT('Ctrl Pts',(0.653841677162244,-2.36655065535509,
1.04129350653413));
#34600=CARTESIAN_POINT('Ctrl Pts',(0.611435398767205,-1.84829648252061,
1.80753169553));
#34601=CARTESIAN_POINT('Ctrl Pts',(0.569029120372168,-1.12642923923531,
2.18058609450059));
#34602=CARTESIAN_POINT('Ctrl Pts',(0.529519413581445,-0.453869321141522,
2.52815891810498));
#34603=CARTESIAN_POINT('Ctrl Pts',(0.490009706790722,0.395437961240758,
2.53442654743051));
#34604=CARTESIAN_POINT('Ctrl Pts',(0.4505,1.07766119456972,2.20539011734829));
#34605=CARTESIAN_POINT('',(0.4505,-1.07508846035129,2.20207516956608));
#34606=CARTESIAN_POINT('Origin',(0.4505,0.,0.));
#34607=CARTESIAN_POINT('Ctrl Pts',(0.4505,-1.07508846035129,2.20207516956608));
#34608=CARTESIAN_POINT('Ctrl Pts',(0.492906278395038,-1.80850750214552,
1.84400821557093));
#34609=CARTESIAN_POINT('Ctrl Pts',(0.535312556790075,-2.34254929575026,
1.09374797713159));
#34610=CARTESIAN_POINT('Ctrl Pts',(0.577718835185113,-2.43734918119715,
0.288262827797322));
#34611=CARTESIAN_POINT('Ctrl Pts',(0.582703391386057,-2.44849223299838,
0.193583781490062));
#34612=CARTESIAN_POINT('Ctrl Pts',(0.587687947587001,-2.45356657398087,
0.0981417296316767));
#34613=CARTESIAN_POINT('Ctrl Pts',(0.592672503787945,-2.45282685237657,
0.00258448634202159));
#34614=CARTESIAN_POINT('Origin',(2.1,0.,0.));
#34615=CARTESIAN_POINT('',(1.50832749621205,-2.4473413370506,0.0014603139898775));
#34616=CARTESIAN_POINT('',(1.39267250378795,-2.44703157660636,0.00122755980643863));
#34617=CARTESIAN_POINT('',(2.1,-2.4505,-3.00099698131059E-16));
#34618=CARTESIAN_POINT('Ctrl Pts',(1.50832749621205,-2.4473413370506,0.0014603139898775));
#34619=CARTESIAN_POINT('Ctrl Pts',(1.49207198636402,-2.44903711369849,0.315247098410422));
#34620=CARTESIAN_POINT('Ctrl Pts',(1.47581647651599,-2.3930852952942,0.628451488488446));
#34621=CARTESIAN_POINT('Ctrl Pts',(1.45956096666796,-2.27670283532662,0.917306581367306));
#34622=CARTESIAN_POINT('Ctrl Pts',(1.41715468827292,-1.97309211847898,1.67085227750118));
#34623=CARTESIAN_POINT('Ctrl Pts',(1.37474840987789,-1.25822153135608,2.25868917842173));
#34624=CARTESIAN_POINT('Ctrl Pts',(1.33234213148285,-0.460215326170196,
2.41101669101588));
#34625=CARTESIAN_POINT('Ctrl Pts',(1.28993585308781,0.337790879015677,2.56334420361003));
#34626=CARTESIAN_POINT('Ctrl Pts',(1.24752957469277,1.21893270226453,2.28016232787779));
#34627=CARTESIAN_POINT('Ctrl Pts',(1.20512329629773,1.77875643166747,1.69141715907579));
#34628=CARTESIAN_POINT('Ctrl Pts',(1.1627170179027,2.33858016107041,1.10267199027379));
#34629=CARTESIAN_POINT('Ctrl Pts',(1.12031073950766,2.57708579662744,0.208363528402023));
#34630=CARTESIAN_POINT('Ctrl Pts',(1.07790446111262,2.384811555813,-0.580950218879841));
#34631=CARTESIAN_POINT('Ctrl Pts',(1.03549818271758,2.19253731499856,-1.3702639661617));
#34632=CARTESIAN_POINT('Ctrl Pts',(0.993091904322546,1.56948319781265,-2.05458299885366));
#34633=CARTESIAN_POINT('Ctrl Pts',(0.950685625927508,0.801608016347805,
-2.3199322416022));
#34634=CARTESIAN_POINT('Ctrl Pts',(0.90827934753247,0.0337328348829553,
-2.58528148435073));
#34635=CARTESIAN_POINT('Ctrl Pts',(0.865873069137432,-0.878963410860835,
-2.43166093715584));
#34636=CARTESIAN_POINT('Ctrl Pts',(0.823466790742394,-1.51750239566356,
-1.92933471230852));
#34637=CARTESIAN_POINT('Ctrl Pts',(0.785087025898947,-2.0954115404323,-1.47470480574751));
#34638=CARTESIAN_POINT('Ctrl Pts',(0.746707261055501,-2.44875466051846,
-0.734445229755698));
#34639=CARTESIAN_POINT('Ctrl Pts',(0.708327496212055,-2.45360913320878,
0.00150472093799672));
#34640=CARTESIAN_POINT('Ctrl Pts',(0.592672503787945,-2.45282685237657,
0.00258448634202159));
#34641=CARTESIAN_POINT('Ctrl Pts',(0.630094225982039,-2.44727336772092,
-0.714814709867619));
#34642=CARTESIAN_POINT('Ctrl Pts',(0.667515948176133,-2.11402153716249,
-1.43870644738133));
#34643=CARTESIAN_POINT('Ctrl Pts',(0.704937670370227,-1.56082513352308,
-1.89496977522306));
#34644=CARTESIAN_POINT('Ctrl Pts',(0.747343948765265,-0.933943223113065,
-2.41200716867997));
#34645=CARTESIAN_POINT('Ctrl Pts',(0.789750227160302,-0.0246214250039735,
-2.58537189536459));
#34646=CARTESIAN_POINT('Ctrl Pts',(0.83215650555534,0.749125781327214,-2.33722376134394));
#34647=CARTESIAN_POINT('Ctrl Pts',(0.874562783950378,1.5228729876584,-2.08907562732328));
#34648=CARTESIAN_POINT('Ctrl Pts',(0.916969062345416,2.16104560221169,-1.41941463259735));
#34649=CARTESIAN_POINT('Ctrl Pts',(0.959375340740454,2.37104638647788,-0.634742664260803));
#34650=CARTESIAN_POINT('Ctrl Pts',(1.00178161913549,2.58104717074407,0.149929304075739));
#34651=CARTESIAN_POINT('Ctrl Pts',(1.04418789753053,2.36287612472317,1.04961224602289));
#34652=CARTESIAN_POINT('Ctrl Pts',(1.08659417592557,1.81650481602726,1.6508958941018));
#34653=CARTESIAN_POINT('Ctrl Pts',(1.1290004543206,1.27013350733135,2.25217954218071));
#34654=CARTESIAN_POINT('Ctrl Pts',(1.17140673271564,0.395561935960428,2.55506389639137));
#34655=CARTESIAN_POINT('Ctrl Pts',(1.21381301111068,-0.405690332469361,
2.42076003474965));
#34656=CARTESIAN_POINT('Ctrl Pts',(1.25621928950572,-1.20694260089915,2.28645617310792));
#34657=CARTESIAN_POINT('Ctrl Pts',(1.29862556790075,-1.9348755663878,1.7149640956138));
#34658=CARTESIAN_POINT('Ctrl Pts',(1.34103184629579,-2.25541184946638,0.968477408375057));
#34659=CARTESIAN_POINT('Ctrl Pts',(1.35824539879318,-2.38552390704169,0.665463603209682));
#34660=CARTESIAN_POINT('Ctrl Pts',(1.37545895129056,-2.44850881837782,0.333615766579194));
#34661=CARTESIAN_POINT('Ctrl Pts',(1.39267250378795,-2.44703157660636,0.00122755980643863));
#34662=CARTESIAN_POINT('Origin',(2.1,0.,0.));
#34663=CARTESIAN_POINT('',(2.30832749621206,-2.44830822615452,-0.00194217634527288));
#34664=CARTESIAN_POINT('',(2.19267250378795,-2.44878095179287,-0.00208303942229182));
#34665=CARTESIAN_POINT('',(2.1,-2.4505,-3.00099698131059E-16));
#34666=CARTESIAN_POINT('Ctrl Pts',(2.30832749621206,-2.44830822615452,-0.00194217634527288));
#34667=CARTESIAN_POINT('Ctrl Pts',(2.27984299006758,-2.44424577234732,0.547360393912042));
#34668=CARTESIAN_POINT('Ctrl Pts',(2.25135848392311,-2.26154082184235,1.09911172701984));
#34669=CARTESIAN_POINT('Ctrl Pts',(2.22287397777864,-1.92217546127181,1.52645421544262));
#34670=CARTESIAN_POINT('Ctrl Pts',(2.1804676993836,-1.41694563966299,2.16265989308967));
#34671=CARTESIAN_POINT('Ctrl Pts',(2.13806142098857,-0.564497850275433,
2.52312911500327));
#34672=CARTESIAN_POINT('Ctrl Pts',(2.09565514259353,0.243894172460438,2.44240461641206));
#34673=CARTESIAN_POINT('Ctrl Pts',(2.05324886419849,1.05228619519631,2.36168011782086));
#34674=CARTESIAN_POINT('Ctrl Pts',(2.01084258580345,1.8166224512805,1.83976189872484));
#34675=CARTESIAN_POINT('Ctrl Pts',(1.96843630740841,2.18606878658389,1.11621194303221));
#34676=CARTESIAN_POINT('Ctrl Pts',(1.92603002901338,2.55551512188727,0.392661987339586));
#34677=CARTESIAN_POINT('Ctrl Pts',(1.88362375061834,2.53007153640987,-0.532519704949663));
#34678=CARTESIAN_POINT('Ctrl Pts',(1.8412174722233,2.12141763927363,-1.23467075668366));
#34679=CARTESIAN_POINT('Ctrl Pts',(1.79881119382826,1.7127637421374,-1.93682180841766));
#34680=CARTESIAN_POINT('Ctrl Pts',(1.75640491543323,0.920899533342334,-2.41594221959641));
#34681=CARTESIAN_POINT('Ctrl Pts',(1.71399863703819,0.109292333967081,-2.45211666963342));
#34682=CARTESIAN_POINT('Ctrl Pts',(1.67159235864315,-0.702314865408171,
-2.48829111967042));
#34683=CARTESIAN_POINT('Ctrl Pts',(1.62918608024811,-1.53366505536361,-2.08151960856568));
#34684=CARTESIAN_POINT('Ctrl Pts',(1.58677980185307,-2.00316472705514,-1.41850660733972));
#34685=CARTESIAN_POINT('Ctrl Pts',(1.56062903330607,-2.29269207328737,-1.00964499073661));
#34686=CARTESIAN_POINT('Ctrl Pts',(1.53447826475906,-2.44461328588265,-0.503338714106133));
#34687=CARTESIAN_POINT('Ctrl Pts',(1.50832749621205,-2.4473413370506,0.0014603139898775));
#34688=CARTESIAN_POINT('Ctrl Pts',(1.39267250378795,-2.44703157660636,0.00122755980643863));
#34689=CARTESIAN_POINT('Ctrl Pts',(1.4178652296856,-2.44486957390303,-0.48523593958517));
#34690=CARTESIAN_POINT('Ctrl Pts',(1.44305795558325,-2.30463286953165,-0.972856884742813));
#34691=CARTESIAN_POINT('Ctrl Pts',(1.46825068148091,-2.03467576323812,-1.37293946448399));
#34692=CARTESIAN_POINT('Ctrl Pts',(1.51065695987595,-1.58026379326277,-2.04638835312089));
#34693=CARTESIAN_POINT('Ctrl Pts',(1.55306323827098,-0.758300252643548,
-2.47180483341132));
#34694=CARTESIAN_POINT('Ctrl Pts',(1.59546951666602,0.0539184165626573,
-2.45395487916923));
#34695=CARTESIAN_POINT('Ctrl Pts',(1.63787579506106,0.866137085768862,-2.43610492492714));
#34696=CARTESIAN_POINT('Ctrl Pts',(1.6802820734561,1.66861088356205,-1.97498853615253));
#34697=CARTESIAN_POINT('Ctrl Pts',(1.72268835185113,2.09300840145503,-1.28224214439752));
#34698=CARTESIAN_POINT('Ctrl Pts',(1.76509463024617,2.51740591934801,-0.589495752642504));
#34699=CARTESIAN_POINT('Ctrl Pts',(1.80750090864121,2.56372715734077,0.334880642092917));
#34700=CARTESIAN_POINT('Ctrl Pts',(1.84990718703624,2.21070701757217,1.06658629749541));
#34701=CARTESIAN_POINT('Ctrl Pts',(1.89231346543128,1.85768687780357,1.79829195289791));
#34702=CARTESIAN_POINT('Ctrl Pts',(1.93471974382632,1.1053253602736,2.33732686896749));
#34703=CARTESIAN_POINT('Ctrl Pts',(1.97712602222136,0.298960721540154,2.43627696427715));
#34704=CARTESIAN_POINT('Ctrl Pts',(2.0195323006164,-0.507403917193297,2.53522705958681));
#34705=CARTESIAN_POINT('Ctrl Pts',(2.06193857901143,-1.36777167713024,2.19409233413654));
#34706=CARTESIAN_POINT('Ctrl Pts',(2.10434485740647,-1.88723228249209,1.56945243436612));
#34707=CARTESIAN_POINT('Ctrl Pts',(2.1337874062003,-2.24789218472075,1.13576687119931));
#34708=CARTESIAN_POINT('Ctrl Pts',(2.16322995499412,-2.44421839872437,0.565418142411997));
#34709=CARTESIAN_POINT('Ctrl Pts',(2.19267250378795,-2.44878095179287,-0.00208303942229182));
#34710=CARTESIAN_POINT('Origin',(2.1,0.,0.));
#34711=CARTESIAN_POINT('',(3.10832749621205,-2.45444621147543,-0.000567327939743623));
#34712=CARTESIAN_POINT('',(2.99267250378795,-2.45452615968528,-0.000257956296186217));
#34713=CARTESIAN_POINT('',(2.1,-2.4505,-3.00099698131059E-16));
#34714=CARTESIAN_POINT('Ctrl Pts',(3.10832749621205,-2.45444621147543,-0.000567327939743623));
#34715=CARTESIAN_POINT('Ctrl Pts',(3.06761399377114,-2.45192087847678,0.779588102337758));
#34716=CARTESIAN_POINT('Ctrl Pts',(3.02690049133023,-2.04779555002706,1.5619550530578));
#34717=CARTESIAN_POINT('Ctrl Pts',(2.98618698888932,-1.40912833240446,2.00973091739006));
#34718=CARTESIAN_POINT('Ctrl Pts',(2.94378071049429,-0.74390676686621,2.47612429607348));
#34719=CARTESIAN_POINT('Ctrl Pts',(2.90137443209925,0.175765592190175,2.57952508637236));
#34720=CARTESIAN_POINT('Ctrl Pts',(2.85896815370421,0.927875800169445,2.27241629395137));
#34721=CARTESIAN_POINT('Ctrl Pts',(2.81656187530917,1.67998600814872,1.96530750153038));
#34722=CARTESIAN_POINT('Ctrl Pts',(2.77415559691413,2.26453406505087,1.24768912638951));
#34723=CARTESIAN_POINT('Ctrl Pts',(2.73174931851909,2.41314815295225,0.448979332617362));
#34724=CARTESIAN_POINT('Ctrl Pts',(2.68934304012406,2.56176224085363,-0.349730461154791));
#34725=CARTESIAN_POINT('Ctrl Pts',(2.64693676172902,2.27444235975423,-1.22953167355824));
#34726=CARTESIAN_POINT('Ctrl Pts',(2.60453048333398,1.68310182647636,-1.78660792355543));
#34727=CARTESIAN_POINT('Ctrl Pts',(2.56212420493894,1.0917612931985,-2.34368417355261));
#34728=CARTESIAN_POINT('Ctrl Pts',(2.51971792654391,0.196400107742168,-2.57803546114354));
#34729=CARTESIAN_POINT('Ctrl Pts',(2.47731164814887,-0.592025137123773,
-2.3820859349775));
#34730=CARTESIAN_POINT('Ctrl Pts',(2.43490536975383,-1.38045038198972,-2.18613640881146));
#34731=CARTESIAN_POINT('Ctrl Pts',(2.39249909135879,-2.06193968626528,-1.55988606888843));
#34732=CARTESIAN_POINT('Ctrl Pts',(2.35009281296376,-2.323678411488,-0.790789832236671));
#34733=CARTESIAN_POINT('Ctrl Pts',(2.33617104071319,-2.40960594532532,-0.538299327276763));
#34734=CARTESIAN_POINT('Ctrl Pts',(2.32224926846262,-2.45029374615601,-0.270413226571201));
#34735=CARTESIAN_POINT('Ctrl Pts',(2.30832749621206,-2.44830822615452,-0.00194217634527288));
#34736=CARTESIAN_POINT('Ctrl Pts',(2.19267250378795,-2.44878095179287,-0.00208303942229182));
#34737=CARTESIAN_POINT('Ctrl Pts',(2.20563623338916,-2.45078987108465,-0.251957189965));
#34738=CARTESIAN_POINT('Ctrl Pts',(2.21859996299037,-2.41562169693219,-0.501279288473224));
#34739=CARTESIAN_POINT('Ctrl Pts',(2.23156369259159,-2.34093495686051,-0.738140446195743));
#34740=CARTESIAN_POINT('Ctrl Pts',(2.27396997098663,-2.09662357508032,-1.51294835289657));
#34741=CARTESIAN_POINT('Ctrl Pts',(2.31637624938166,-1.42944736073319,-2.15441909220764));
#34742=CARTESIAN_POINT('Ctrl Pts',(2.3587825277767,-0.645643695495165,-2.36811546388376));
#34743=CARTESIAN_POINT('Ctrl Pts',(2.40118880617174,0.138159969742868,-2.58181183555988));
#34744=CARTESIAN_POINT('Ctrl Pts',(2.44359508456678,1.0385910858718,-2.36773383960104));
#34745=CARTESIAN_POINT('Ctrl Pts',(2.48600136296181,1.64235124726471,-1.82414509847746));
#34746=CARTESIAN_POINT('Ctrl Pts',(2.52840764135685,2.24611140865762,-1.28055635735387));
#34747=CARTESIAN_POINT('Ctrl Pts',(2.57081391975189,2.55320061531452,-0.407456871065538));
#34748=CARTESIAN_POINT('Ctrl Pts',(2.61322019814693,2.42265969342523,0.394400630578321));
#34749=CARTESIAN_POINT('Ctrl Pts',(2.65562647654196,2.29211877153594,1.19625813222218));
#34750=CARTESIAN_POINT('Ctrl Pts',(2.698032754937,1.72394772110046,1.92687364922157));
#34751=CARTESIAN_POINT('Ctrl Pts',(2.74043903333204,0.978946913942611,2.25088694187707));
#34752=CARTESIAN_POINT('Ctrl Pts',(2.78284531172708,0.233946106784758,2.57490023453258));
#34753=CARTESIAN_POINT('Ctrl Pts',(2.82525159012211,-0.687884457095468,
2.4923113028442));
#34754=CARTESIAN_POINT('Ctrl Pts',(2.86765786851715,-1.36343705087406,2.04103923356386));
#34755=CARTESIAN_POINT('Ctrl Pts',(2.90932941360742,-2.02728498655577,1.59758592677255));
#34756=CARTESIAN_POINT('Ctrl Pts',(2.95100095869768,-2.45331507036201,0.798114451695043));
#34757=CARTESIAN_POINT('Ctrl Pts',(2.99267250378795,-2.45452615968528,-0.000257956296186217));
#34758=CARTESIAN_POINT('Origin',(-1.02854511860477,0.,0.));
#34759=CARTESIAN_POINT('',(3.37145488139523,-1.99796228538691,-0.000461814898120527));
#34760=CARTESIAN_POINT('',(3.52954511860477,-1.99388364589384,0.00171352076686206));
#34761=CARTESIAN_POINT('',(-1.02854511860477,-1.99475,-1.3903373121373E-14));
#34762=CARTESIAN_POINT('',(3.7495,1.96855338775712,-0.342146149675743));
#34763=CARTESIAN_POINT('Ctrl Pts',(3.37145488139523,-1.9979622853869,-0.00046181489812086));
#34764=CARTESIAN_POINT('Ctrl Pts',(3.37314765734935,-1.99804775533437,-0.0268661915402383));
#34765=CARTESIAN_POINT('Ctrl Pts',(3.41724671169852,-1.98555193750958,-0.714654081742635));
#34766=CARTESIAN_POINT('Ctrl Pts',(3.50375204444272,-1.19567276206334,-2.03345149280708));
#34767=CARTESIAN_POINT('Ctrl Pts',(3.62807430802352,1.01077702469923,-2.10391583542276));
#34768=CARTESIAN_POINT('Ctrl Pts',(3.70999029320928,1.8598858594405,-0.9490459619713));
#34769=CARTESIAN_POINT('Ctrl Pts',(3.7495,1.96858208699144,-0.342145191103274));
#34770=CARTESIAN_POINT('',(3.7495,0.311349471200418,-1.97030177112117));
#34771=CARTESIAN_POINT('Origin',(3.7495,0.,0.));
#34772=CARTESIAN_POINT('Ctrl Pts',(3.52954511860477,-1.99388364589384,0.00171352076686202));
#34773=CARTESIAN_POINT('Ctrl Pts',(3.56045713400815,-1.98914408542672,-0.483238452536014));
#34774=CARTESIAN_POINT('Ctrl Pts',(3.63377542780655,-1.56621865433236,-1.64019501966093));
#34775=CARTESIAN_POINT('Ctrl Pts',(3.70709372160496,-0.344875555534673,
-2.07399924429869));
#34776=CARTESIAN_POINT('Ctrl Pts',(3.7495,0.311349471200418,-1.97030177112117));
#34777=CARTESIAN_POINT('Origin',(-1.02854511860477,0.,0.));
#34778=CARTESIAN_POINT('',(2.57145488139523,-1.99296585762976,-0.00158096562527621));
#34779=CARTESIAN_POINT('',(2.72954511860477,-1.99802736463261,-0.000209980951578204));
#34780=CARTESIAN_POINT('',(-1.02854511860477,-1.99475,-1.3903373121373E-14));
#34781=CARTESIAN_POINT('Ctrl Pts',(2.57145488139523,-1.99296585762976,-0.00158096562527653));
#34782=CARTESIAN_POINT('Ctrl Pts',(2.58537665364579,-1.99458210575176,-0.22012111148864));
#34783=CARTESIAN_POINT('Ctrl Pts',(2.6417047042914,-1.86057489097072,-1.10241677508306));
#34784=CARTESIAN_POINT('Ctrl Pts',(2.74043903333204,-0.568966582236417,
-2.28933216365562));
#34785=CARTESIAN_POINT('Ctrl Pts',(2.86765786851715,1.61755256653611,-1.71703398256359));
#34786=CARTESIAN_POINT('Ctrl Pts',(2.99487670370227,2.31920284136536,0.43148689290074));
#34787=CARTESIAN_POINT('Ctrl Pts',(3.12209553888738,0.891705714445654,2.18394874208935));
#34788=CARTESIAN_POINT('Ctrl Pts',(3.24762159811837,-1.32429877248386,1.93479847352036));
#34789=CARTESIAN_POINT('Ctrl Pts',(3.33074137895432,-1.99590662001288,0.634598395077826));
#34790=CARTESIAN_POINT('Ctrl Pts',(3.37145488139523,-1.9979622853869,-0.00046181489812086));
#34791=CARTESIAN_POINT('Ctrl Pts',(2.72954511860477,-1.99802736463261,-0.000209980951578455));
#34792=CARTESIAN_POINT('Ctrl Pts',(2.73027985190955,-1.99804474664541,-0.0116685242216074));
#34793=CARTESIAN_POINT('Ctrl Pts',(2.77342086360936,-1.99275319078551,-0.684458429783003));
#34794=CARTESIAN_POINT('Ctrl Pts',(2.85896815370421,-1.24161073233134,-2.00578545294822));
#34795=CARTESIAN_POINT('Ctrl Pts',(2.98618698888932,1.01505102673121,-2.12930526437765));
#34796=CARTESIAN_POINT('Ctrl Pts',(3.11340582407443,2.34023742749476,-0.298347997134086));
#34797=CARTESIAN_POINT('Ctrl Pts',(3.24062465925955,1.51640407537933,1.80695219210931));
#34798=CARTESIAN_POINT('Ctrl Pts',(3.36784349444466,-0.698217180620254,
2.25257951257453));
#34799=CARTESIAN_POINT('Ctrl Pts',(3.4641503142264,-1.8913724236262,1.02579681025012));
#34800=CARTESIAN_POINT('Ctrl Pts',(3.51805085561311,-1.99564599473338,0.182037108431196));
#34801=CARTESIAN_POINT('Ctrl Pts',(3.52954511860477,-1.99388364589384,0.00171352076686202));
#34802=CARTESIAN_POINT('Origin',(-1.02854511860477,0.,0.));
#34803=CARTESIAN_POINT('',(1.77145488139523,-1.99217879293274,0.0011887212125215));
#34804=CARTESIAN_POINT('',(1.92954511860477,-1.9933506645945,-0.0016956306417637));
#34805=CARTESIAN_POINT('',(-1.02854511860477,-1.99475,-1.3903373121373E-14));
#34806=CARTESIAN_POINT('Ctrl Pts',(1.77145488139523,-1.99217879293274,0.00118872121252139));
#34807=CARTESIAN_POINT('Ctrl Pts',(1.79760564994223,-1.98995811141171,-0.409726545587932));
#34808=CARTESIAN_POINT('Ctrl Pts',(1.86616269688428,-1.66575302028294,-1.49020154805744));
#34809=CARTESIAN_POINT('Ctrl Pts',(1.97712602222136,0.105037018421004,-2.35663178238676));
#34810=CARTESIAN_POINT('Ctrl Pts',(2.10434485740647,2.03881110186596,-1.18659451627925));
#34811=CARTESIAN_POINT('Ctrl Pts',(2.23156369259159,2.1009456770111,1.07274787999985));
#34812=CARTESIAN_POINT('Ctrl Pts',(2.3587825277767,0.234396303221342,2.34729964601711));
#34813=CARTESIAN_POINT('Ctrl Pts',(2.47207959071125,-1.61951967361292,1.56334588605397));
#34814=CARTESIAN_POINT('Ctrl Pts',(2.54297037525076,-1.98965894894504,0.445560965417686));
#34815=CARTESIAN_POINT('Ctrl Pts',(2.57145488139523,-1.99296585762976,-0.00158096562527653));
#34816=CARTESIAN_POINT('Ctrl Pts',(1.92954511860477,-1.9933506645945,-0.00169563064176386));
#34817=CARTESIAN_POINT('Ctrl Pts',(1.94250884820599,-1.9949859601494,-0.205097573835013));
#34818=CARTESIAN_POINT('Ctrl Pts',(1.99787885620224,-1.87271362382115,-1.0719380117463));
#34819=CARTESIAN_POINT('Ctrl Pts',(2.09565514259353,-0.620502089064916,
-2.27590338356333));
#34820=CARTESIAN_POINT('Ctrl Pts',(2.22287397777864,1.57839809730298,-1.75311364786995));
#34821=CARTESIAN_POINT('Ctrl Pts',(2.35009281296375,2.32832610584676,0.379041259626889));
#34822=CARTESIAN_POINT('Ctrl Pts',(2.47731164814887,0.940822490842265,2.16324281343369));
#34823=CARTESIAN_POINT('Ctrl Pts',(2.60379575002921,-1.29733504359323,1.96272110482245));
#34824=CARTESIAN_POINT('Ctrl Pts',(2.68787357351451,-1.99704151667196,0.649679168544651));
#34825=CARTESIAN_POINT('Ctrl Pts',(2.72954511860477,-1.99802736463261,-0.000209980951578455));
#34826=CARTESIAN_POINT('Origin',(-1.02854511860477,0.,0.));
#34827=CARTESIAN_POINT('',(0.971454881395227,-1.99728088898928,0.00122486924751956));
#34828=CARTESIAN_POINT('',(1.12954511860477,-1.99192664249562,0.000999255222959294));
#34829=CARTESIAN_POINT('',(-1.02854511860477,-1.99475,-1.3903373121373E-14));
#34830=CARTESIAN_POINT('Ctrl Pts',(0.971454881395227,-1.99728088898927,
0.00122486924751962));
#34831=CARTESIAN_POINT('Ctrl Pts',(1.00983464623867,-1.99332926303579,-0.597851304654232));
#34832=CARTESIAN_POINT('Ctrl Pts',(1.09062068947716,-1.38789856934239,-1.86623844205377));
#34833=CARTESIAN_POINT('Ctrl Pts',(1.21381301111068,0.770409879037013,-2.22951431439528));
#34834=CARTESIAN_POINT('Ctrl Pts',(1.34103184629579,2.2919408322179,-0.558371212421443));
#34835=CARTESIAN_POINT('Ctrl Pts',(1.4682506814809,1.70949751469815,1.62557712993974));
#34836=CARTESIAN_POINT('Ctrl Pts',(1.59546951666602,-0.442297203023523,
2.3171221778282));
#34837=CARTESIAN_POINT('Ctrl Pts',(1.69653758330413,-1.82919670899801,1.17667700891804));
#34838=CARTESIAN_POINT('Ctrl Pts',(1.7551993715472,-1.99355918488066,0.256616669885401));
#34839=CARTESIAN_POINT('Ctrl Pts',(1.77145488139523,-1.99217879293274,0.00118872121252139));
#34840=CARTESIAN_POINT('Ctrl Pts',(1.12954511860477,-1.99192664249562,0.000999255222959156));
#34841=CARTESIAN_POINT('Ctrl Pts',(1.15473784450243,-1.99016673435751,-0.394990569470533));
#34842=CARTESIAN_POINT('Ctrl Pts',(1.22233684879512,-1.68385713906353,-1.46006818262196));
#34843=CARTESIAN_POINT('Ctrl Pts',(1.33234213148285,0.0518230335398809,
-2.35838898816837));
#34844=CARTESIAN_POINT('Ctrl Pts',(1.45956096666796,2.01150629183162,-1.23231849254524));
#34845=CARTESIAN_POINT('Ctrl Pts',(1.58677980185307,2.12462519346728,1.02505732471468));
#34846=CARTESIAN_POINT('Ctrl Pts',(1.71399863703819,0.287318761604926,2.341408965804));
#34847=CARTESIAN_POINT('Ctrl Pts',(1.82825374262209,-1.59964409149406,1.59323058813681));
#34848=CARTESIAN_POINT('Ctrl Pts',(1.90010256981095,-1.98963666633563,0.46026028956389));
#34849=CARTESIAN_POINT('Ctrl Pts',(1.92954511860477,-1.9933506645945,-0.00169563064176386));
#34850=CARTESIAN_POINT('Origin',(3.7495,5.69858952725515E-16,8.58067791224701E-17));
#34851=CARTESIAN_POINT('',(3.7495,-0.778675485261968,2.32349192782158));
#34852=CARTESIAN_POINT('Ctrl Pts',(3.7495,1.96858208699144,-0.342145191103275));
#34853=CARTESIAN_POINT('Ctrl Pts',(3.7495,1.9815616872834,-0.298310884910423));
#34854=CARTESIAN_POINT('Ctrl Pts',(3.7495,1.99290809419775,-0.254078248249005));
#34855=CARTESIAN_POINT('Ctrl Pts',(3.7495,2.00257142811677,-0.209519371139262));
#34856=CARTESIAN_POINT('Ctrl Pts',(3.7495,2.01774911827413,-0.139533087295686));
#34857=CARTESIAN_POINT('Ctrl Pts',(3.7495,2.02877766589333,-0.0687429867827845));
#34858=CARTESIAN_POINT('Ctrl Pts',(3.7495,2.0358403959562,0.00254783820095801));
#34859=CARTESIAN_POINT('Ctrl Pts',(3.7495,2.03975568900501,0.0420685998636354));
#34860=CARTESIAN_POINT('Ctrl Pts',(3.7495,2.04245137734559,0.0817436825706553));
#34861=CARTESIAN_POINT('Ctrl Pts',(3.7495,2.04395245361958,0.121523911179525));
#34862=CARTESIAN_POINT('Ctrl Pts',(3.7495,2.04469239255816,0.14113313467024));
#34863=CARTESIAN_POINT('Ctrl Pts',(3.7495,2.04514198673599,0.1607679282988));
#34864=CARTESIAN_POINT('Ctrl Pts',(3.7495,2.04530383971613,0.180422499284288));
#34865=CARTESIAN_POINT('Ctrl Pts',(3.7495,2.04542150599878,0.194711271125375));
#34866=CARTESIAN_POINT('Ctrl Pts',(3.7495,2.04538700750185,0.209000770084867));
#34867=CARTESIAN_POINT('Ctrl Pts',(3.7495,2.04520188976334,0.223288377519502));
#34868=CARTESIAN_POINT('Ctrl Pts',(3.7495,2.04422777843955,0.298471449137185));
#34869=CARTESIAN_POINT('Ctrl Pts',(3.7495,2.03908721806814,0.373602904565653));
#34870=CARTESIAN_POINT('Ctrl Pts',(3.7495,2.02997465441022,0.448351081788569));
#34871=CARTESIAN_POINT('Ctrl Pts',(3.7495,2.02256734831719,0.509111439616568));
#34872=CARTESIAN_POINT('Ctrl Pts',(3.7495,2.01253450727956,0.569619224635133));
#34873=CARTESIAN_POINT('Ctrl Pts',(3.7495,1.99995593276109,0.629702334442525));
#34874=CARTESIAN_POINT('Ctrl Pts',(3.7495,1.99497851113414,0.653477601642343));
#34875=CARTESIAN_POINT('Ctrl Pts',(3.7495,1.98960223154056,0.677186401041374));
#34876=CARTESIAN_POINT('Ctrl Pts',(3.7495,1.98383111448107,0.700818115169424));
#34877=CARTESIAN_POINT('Ctrl Pts',(3.7495,1.9797346628459,0.717592367534078));
#34878=CARTESIAN_POINT('Ctrl Pts',(3.7495,1.97543835661824,0.73433067219556));
#34879=CARTESIAN_POINT('Ctrl Pts',(3.7495,1.97095036387965,0.75100507213264));
#34880=CARTESIAN_POINT('Ctrl Pts',(3.7495,1.95073133439056,0.826125555537453));
#34881=CARTESIAN_POINT('Ctrl Pts',(3.7495,1.92660313283638,0.900047712653736));
#34882=CARTESIAN_POINT('Ctrl Pts',(3.7495,1.89876242591588,0.972434182739083));
#34883=CARTESIAN_POINT('Ctrl Pts',(3.7495,1.87039439526001,1.0461917065087));
#34884=CARTESIAN_POINT('Ctrl Pts',(3.7495,1.83817184686105,1.11835584035847));
#34885=CARTESIAN_POINT('Ctrl Pts',(3.7495,1.80224930993342,1.18857395679423));
#34886=CARTESIAN_POINT('Ctrl Pts',(3.7495,1.7760002690807,1.23988320064403));
#34887=CARTESIAN_POINT('Ctrl Pts',(3.7495,1.74777452061065,1.29015354758491));
#34888=CARTESIAN_POINT('Ctrl Pts',(3.7495,1.71761511908426,1.33924389352241));
#34889=CARTESIAN_POINT('Ctrl Pts',(3.7495,1.69499556793946,1.37606165297554));
#34890=CARTESIAN_POINT('Ctrl Pts',(3.7495,1.67128803582605,1.41221561571887));
#34891=CARTESIAN_POINT('Ctrl Pts',(3.7495,1.64650557338506,1.44764383520813));
#34892=CARTESIAN_POINT('Ctrl Pts',(3.7495,1.63899129825552,1.4583860037568));
#34893=CARTESIAN_POINT('Ctrl Pts',(3.7495,1.63137694759429,1.46906310763164));
#34894=CARTESIAN_POINT('Ctrl Pts',(3.7495,1.62366670212987,1.47966802512963));
#34895=CARTESIAN_POINT('Ctrl Pts',(3.7495,1.57597942677249,1.54525862444354));
#34896=CARTESIAN_POINT('Ctrl Pts',(3.7495,1.5247886717997,1.60787005386699));
#34897=CARTESIAN_POINT('Ctrl Pts',(3.7495,1.47026968124208,1.66714346245527));
#34898=CARTESIAN_POINT('Ctrl Pts',(3.7495,1.44638830509851,1.69310745319189));
#34899=CARTESIAN_POINT('Ctrl Pts',(3.7495,1.42186764705416,1.71843085924667));
#34900=CARTESIAN_POINT('Ctrl Pts',(3.7495,1.39671939232244,1.74308270436089));
#34901=CARTESIAN_POINT('Ctrl Pts',(3.7495,1.34130534744921,1.79740291329546));
#34902=CARTESIAN_POINT('Ctrl Pts',(3.7495,1.28284699014363,1.8484646870851));
#34903=CARTESIAN_POINT('Ctrl Pts',(3.7495,1.22168664345893,1.89625311771161));
#34904=CARTESIAN_POINT('Ctrl Pts',(3.7495,1.15924467146654,1.94504296290533));
#34905=CARTESIAN_POINT('Ctrl Pts',(3.7495,1.09398565883421,1.99042130918484));
#34906=CARTESIAN_POINT('Ctrl Pts',(3.7495,1.02623383171228,2.03233611927841));
#34907=CARTESIAN_POINT('Ctrl Pts',(3.7495,1.01504933682572,2.03925543052176));
#34908=CARTESIAN_POINT('Ctrl Pts',(3.7495,1.00379683470936,2.04608026748763));
#34909=CARTESIAN_POINT('Ctrl Pts',(3.7495,0.992477701009896,2.05281028972857));
#34910=CARTESIAN_POINT('Ctrl Pts',(3.7495,0.98172367113139,2.05920431794519));
#34911=CARTESIAN_POINT('Ctrl Pts',(3.7495,0.970918002482417,2.0655077016547));
#34912=CARTESIAN_POINT('Ctrl Pts',(3.7495,0.960062601834612,2.07172027426472));
#34913=CARTESIAN_POINT('Ctrl Pts',(3.7495,0.889742058929685,2.11196489470268));
#34914=CARTESIAN_POINT('Ctrl Pts',(3.7495,0.817332785201951,2.1484046376665));
#34915=CARTESIAN_POINT('Ctrl Pts',(3.7495,0.743220237068545,2.18103885646569));
#34916=CARTESIAN_POINT('Ctrl Pts',(3.7495,0.667662831350121,2.21430929409355));
#34917=CARTESIAN_POINT('Ctrl Pts',(3.7495,0.590334370784013,2.24362483808424));
#34918=CARTESIAN_POINT('Ctrl Pts',(3.7495,0.511603026210655,2.26894693390449));
#34919=CARTESIAN_POINT('Ctrl Pts',(3.7495,0.432317848910233,2.29444715706982));
#34920=CARTESIAN_POINT('Ctrl Pts',(3.7495,0.351609102256153,2.31589797265474));
#34921=CARTESIAN_POINT('Ctrl Pts',(3.7495,0.269824604998954,2.33321541018852));
#34922=CARTESIAN_POINT('Ctrl Pts',(3.7495,0.237358854089674,2.34008986234283));
#34923=CARTESIAN_POINT('Ctrl Pts',(3.7495,0.204723346095625,2.34631243924816));
#34924=CARTESIAN_POINT('Ctrl Pts',(3.7495,0.171939102120644,2.35187572830449));
#34925=CARTESIAN_POINT('Ctrl Pts',(3.7495,0.155509674618924,2.35466370335408));
#34926=CARTESIAN_POINT('Ctrl Pts',(3.7495,0.139039506256638,2.35728648113795));
#34927=CARTESIAN_POINT('Ctrl Pts',(3.7495,0.122556884830378,2.35973950905647));
#34928=CARTESIAN_POINT('Ctrl Pts',(3.7495,0.0376196930479621,2.3723802958206));
#34929=CARTESIAN_POINT('Ctrl Pts',(3.7495,-0.0477770629941537,2.38054113558466));
#34930=CARTESIAN_POINT('Ctrl Pts',(3.7495,-0.133242592282125,2.38419061215778));
#34931=CARTESIAN_POINT('Ctrl Pts',(3.7495,-0.21883889220705,2.38784567278777));
#34932=CARTESIAN_POINT('Ctrl Pts',(3.7495,-0.304505141737865,2.38697591690384));
#34933=CARTESIAN_POINT('Ctrl Pts',(3.7495,-0.389871608999167,2.38150287230091));
#34934=CARTESIAN_POINT('Ctrl Pts',(3.7495,-0.473426854966115,2.37614594934677));
#34935=CARTESIAN_POINT('Ctrl Pts',(3.7495,-0.55669585319343,2.36637916882364));
#34936=CARTESIAN_POINT('Ctrl Pts',(3.7495,-0.639339556196431,2.35208041838678));
#34937=CARTESIAN_POINT('Ctrl Pts',(3.7495,-0.686004718048208,2.34400656061943));
#34938=CARTESIAN_POINT('Ctrl Pts',(3.7495,-0.732470576108049,2.33448685588941));
#34939=CARTESIAN_POINT('Ctrl Pts',(3.7495,-0.778675485261984,2.32349192782157));
#34940=CARTESIAN_POINT('',(3.7495,-2.4505,-3.00099698131059E-16));
#34941=CARTESIAN_POINT('Origin',(3.7495,0.,0.));
#34942=CARTESIAN_POINT('',(3.7495,-2.31305386802746,0.815353369809073));
#34943=CARTESIAN_POINT('Origin',(3.7495,0.,0.));
#34944=CARTESIAN_POINT('Ctrl Pts',(3.7495,-2.31513335459631,0.81563149263664));
#34945=CARTESIAN_POINT('Ctrl Pts',(3.7495,-2.32908511219393,0.761794304485864));
#34946=CARTESIAN_POINT('Ctrl Pts',(3.7495,-2.34105243639297,0.707526344258663));
#34947=CARTESIAN_POINT('Ctrl Pts',(3.7495,-2.35095796922772,0.652895508310378));
#34948=CARTESIAN_POINT('Ctrl Pts',(3.7495,-2.36615894451881,0.569059332989447));
#34949=CARTESIAN_POINT('Ctrl Pts',(3.7495,-2.37650681260459,0.484368010711472));
#34950=CARTESIAN_POINT('Ctrl Pts',(3.7495,-2.38213543171266,0.399197491499006));
#34951=CARTESIAN_POINT('Ctrl Pts',(3.7495,-2.38498599869696,0.356063595699415));
#34952=CARTESIAN_POINT('Ctrl Pts',(3.7495,-2.38662532033442,0.312806868142191));
#34953=CARTESIAN_POINT('Ctrl Pts',(3.7495,-2.38706590699035,0.269477264460517));
#34954=CARTESIAN_POINT('Ctrl Pts',(3.7495,-2.38734080394354,0.242442455587761));
#34955=CARTESIAN_POINT('Ctrl Pts',(3.7495,-2.38714897815231,0.215379296141133));
#34956=CARTESIAN_POINT('Ctrl Pts',(3.7495,-2.38649286933422,0.18830018295618));
#34957=CARTESIAN_POINT('Ctrl Pts',(3.7495,-2.38607609390504,0.171098906722011));
#34958=CARTESIAN_POINT('Ctrl Pts',(3.7495,-2.3854721526339,0.153900233382592));
#34959=CARTESIAN_POINT('Ctrl Pts',(3.7495,-2.38468248454918,0.136712098302334));
#34960=CARTESIAN_POINT('Ctrl Pts',(3.7495,-2.38078339237081,0.0518433738995889));
#34961=CARTESIAN_POINT('Ctrl Pts',(3.7495,-2.37235943327698,-0.032807596098823));
#34962=CARTESIAN_POINT('Ctrl Pts',(3.7495,-2.35953861383588,-0.116866026728083));
#34963=CARTESIAN_POINT('Ctrl Pts',(3.7495,-2.34969292129715,-0.181418333003472));
#34964=CARTESIAN_POINT('Ctrl Pts',(3.7495,-2.337253079783,-0.245621176759048));
#34965=CARTESIAN_POINT('Ctrl Pts',(3.7495,-2.32225795639588,-0.309296437066621));
#34966=CARTESIAN_POINT('Ctrl Pts',(3.7495,-2.31481601340137,-0.340897888094137));
#34967=CARTESIAN_POINT('Ctrl Pts',(3.7495,-2.3067444494143,-0.372369249750108));
#34968=CARTESIAN_POINT('Ctrl Pts',(3.7495,-2.29804664763249,-0.403687743159158));
#34969=CARTESIAN_POINT('Ctrl Pts',(3.7495,-2.2928307316521,-0.422468882848428));
#34970=CARTESIAN_POINT('Ctrl Pts',(3.7495,-2.28738798603973,-0.441199905116059));
#34971=CARTESIAN_POINT('Ctrl Pts',(3.7495,-2.28172827744347,-0.459846435299733));
#34972=CARTESIAN_POINT('Ctrl Pts',(3.7495,-2.25757253969978,-0.539430160377721));
#34973=CARTESIAN_POINT('Ctrl Pts',(3.7495,-2.22944528228881,-0.617567924839354));
#34974=CARTESIAN_POINT('Ctrl Pts',(3.7495,-2.19746473876446,-0.693910868197669));
#34975=CARTESIAN_POINT('Ctrl Pts',(3.7495,-2.16615935321421,-0.76864209576586));
#34976=CARTESIAN_POINT('Ctrl Pts',(3.7495,-2.13116109945797,-0.84165425052456));
#34977=CARTESIAN_POINT('Ctrl Pts',(3.7495,-2.09254034740989,-0.912592837701785));
#34978=CARTESIAN_POINT('Ctrl Pts',(3.7495,-2.05476766251083,-0.981973695363329));
#34979=CARTESIAN_POINT('Ctrl Pts',(3.7495,-2.01352934821663,-1.04937167195347));
#34980=CARTESIAN_POINT('Ctrl Pts',(3.7495,-1.96885960929661,-1.11441869429856));
#34981=CARTESIAN_POINT('Ctrl Pts',(3.7495,-1.95318632744929,-1.13724175839501));
#34982=CARTESIAN_POINT('Ctrl Pts',(3.7495,-1.93709034646413,-1.1597750203898));
#34983=CARTESIAN_POINT('Ctrl Pts',(3.7495,-1.92057235305432,-1.18200127152593));
#34984=CARTESIAN_POINT('Ctrl Pts',(3.7495,-1.91106338439778,-1.19479633204945));
#34985=CARTESIAN_POINT('Ctrl Pts',(3.7495,-1.90141455374021,-1.20748963577181));
#34986=CARTESIAN_POINT('Ctrl Pts',(3.7495,-1.8916259361486,-1.22007778499248));
#34987=CARTESIAN_POINT('Ctrl Pts',(3.7495,-1.88396079263015,-1.22993514937567));
#34988=CARTESIAN_POINT('Ctrl Pts',(3.7495,-1.87621545865249,-1.23972090682631));
#34989=CARTESIAN_POINT('Ctrl Pts',(3.7495,-1.86839145414301,-1.24943232120233));
#34990=CARTESIAN_POINT('Ctrl Pts',(3.7495,-1.81941381572349,-1.31022499345529));
#34991=CARTESIAN_POINT('Ctrl Pts',(3.7495,-1.76734121286946,-1.36812667523011));
#34992=CARTESIAN_POINT('Ctrl Pts',(3.7495,-1.71224095284068,-1.42281218692403));
#34993=CARTESIAN_POINT('Ctrl Pts',(3.7495,-1.69359197104109,-1.44132079490062));
#34994=CARTESIAN_POINT('Ctrl Pts',(3.7495,-1.67459588005271,-1.45946065497124));
#34995=CARTESIAN_POINT('Ctrl Pts',(3.7495,-1.65525445681708,-1.4772180716962));
#34996=CARTESIAN_POINT('Ctrl Pts',(3.7495,-1.59693556290941,-1.53076081720367));
#34997=CARTESIAN_POINT('Ctrl Pts',(3.7495,-1.53547843782113,-1.58083011632459));
#34998=CARTESIAN_POINT('Ctrl Pts',(3.7495,-1.47124006561597,-1.62733004442714));
#34999=CARTESIAN_POINT('Ctrl Pts',(3.7495,-1.40824533562139,-1.67292974309684));
#35000=CARTESIAN_POINT('Ctrl Pts',(3.7495,-1.34257497746214,-1.71509694250743));
#35001=CARTESIAN_POINT('Ctrl Pts',(3.7495,-1.27455552459032,-1.75369441034441));
#35002=CARTESIAN_POINT('Ctrl Pts',(3.7495,-1.25783784098724,-1.76318081795188));
#35003=CARTESIAN_POINT('Ctrl Pts',(3.7495,-1.24097196291893,-1.77245454468573));
#35004=CARTESIAN_POINT('Ctrl Pts',(3.7495,-1.2239962012115,-1.78149579204408));
#35005=CARTESIAN_POINT('Ctrl Pts',(3.7495,-1.15532479262889,-1.818070008986));
#35006=CARTESIAN_POINT('Ctrl Pts',(3.7495,-1.0847804637132,-1.85089071870811));
#35007=CARTESIAN_POINT('Ctrl Pts',(3.7495,-1.01271311544069,-1.87989331065926));
#35008=CARTESIAN_POINT('Ctrl Pts',(3.7495,-0.940712023936066,-1.90886923841299));
#35009=CARTESIAN_POINT('Ctrl Pts',(3.7495,-0.867189652651409,-1.9340341824166));
#35010=CARTESIAN_POINT('Ctrl Pts',(3.7495,-0.792485063082482,-1.95527294001421));
#35011=CARTESIAN_POINT('Ctrl Pts',(3.7495,-0.719036476900967,-1.97615461176689));
#35012=CARTESIAN_POINT('Ctrl Pts',(3.7495,-0.644444141266421,-1.99324098626649));
#35013=CARTESIAN_POINT('Ctrl Pts',(3.7495,-0.56903562000595,-2.00637298650572));
#35014=CARTESIAN_POINT('Ctrl Pts',(3.7495,-0.540403830116529,-2.01135906321685));
#35015=CARTESIAN_POINT('Ctrl Pts',(3.7495,-0.511654504155911,-2.0157745477122));
#35016=CARTESIAN_POINT('Ctrl Pts',(3.7495,-0.482806204745629,-2.01960882217606));
#35017=CARTESIAN_POINT('Ctrl Pts',(3.7495,-0.470508509360357,-2.02124332890068));
#35018=CARTESIAN_POINT('Ctrl Pts',(3.7495,-0.458192645595391,-2.0227721434037));
#35019=CARTESIAN_POINT('Ctrl Pts',(3.7495,-0.445874680385831,-2.02419294658075));
#35020=CARTESIAN_POINT('Ctrl Pts',(3.7495,-0.371370875225623,-2.03278651226092));
#35021=CARTESIAN_POINT('Ctrl Pts',(3.7495,-0.29665767767233,-2.03745123135788));
#35022=CARTESIAN_POINT('Ctrl Pts',(3.7495,-0.222044113785007,-2.03809073316757));
#35023=CARTESIAN_POINT('Ctrl Pts',(3.7495,-0.148642426162284,-2.03871984816521));
#35024=CARTESIAN_POINT('Ctrl Pts',(3.7495,-0.0753363029714272,-2.03545337277455));
#35025=CARTESIAN_POINT('Ctrl Pts',(3.7495,-0.00243027506051708,-2.02815091108686));
#35026=CARTESIAN_POINT('Ctrl Pts',(3.7495,0.0681397525587181,-2.02108242940222));
#35027=CARTESIAN_POINT('Ctrl Pts',(3.7495,0.138335550220238,-2.01023226935319));
#35028=CARTESIAN_POINT('Ctrl Pts',(3.7495,0.207860443914689,-1.99542917781665));
#35029=CARTESIAN_POINT('Ctrl Pts',(3.7495,0.242537247572915,-1.98804586701285));
#35030=CARTESIAN_POINT('Ctrl Pts',(3.7495,0.277046768135923,-1.97967850842822));
#35031=CARTESIAN_POINT('Ctrl Pts',(3.7495,0.311349471200403,-1.97030177112117));
#35032=CARTESIAN_POINT('Ctrl Pts',(0.187372614816828,-0.875140871775444,
1.79252782880716));
#35033=CARTESIAN_POINT('Ctrl Pts',(0.229778893211866,-1.47215684142207,
1.50105504509697));
#35034=CARTESIAN_POINT('Ctrl Pts',(0.314591450001942,-2.34159562354249,
0.279605046625738));
#35035=CARTESIAN_POINT('Ctrl Pts',(0.441810285187055,-1.5004500718559,-1.82229423022658));
#35036=CARTESIAN_POINT('Ctrl Pts',(0.569029120372168,0.720161627933661,
-2.24566001911148));
#35037=CARTESIAN_POINT('Ctrl Pts',(0.696247955557281,2.27861274755843,-0.610312617483778));
#35038=CARTESIAN_POINT('Ctrl Pts',(0.823466790742394,1.74582756814582,1.5867604881466));
#35039=CARTESIAN_POINT('Ctrl Pts',(0.950685625927508,-0.389922248616644,
2.3264200256635));
#35040=CARTESIAN_POINT('Ctrl Pts',(1.07790446111262,-2.16757287041851,0.930806287755246));
#35041=CARTESIAN_POINT('Ctrl Pts',(1.20512329629774,-1.95545520271826,-1.31949954838954));
#35042=CARTESIAN_POINT('Ctrl Pts',(1.33234213148285,0.0518230335398809,
-2.35838898816837));
#35043=CARTESIAN_POINT('Ctrl Pts',(1.45956096666796,2.01150629183162,-1.23231849254524));
#35044=CARTESIAN_POINT('Ctrl Pts',(1.58677980185307,2.12462519346728,1.02505732471468));
#35045=CARTESIAN_POINT('Ctrl Pts',(1.71399863703819,0.287318761604926,2.341408965804));
#35046=CARTESIAN_POINT('Ctrl Pts',(1.8412174722233,-1.8137445999142,1.50834000813179));
#35047=CARTESIAN_POINT('Ctrl Pts',(1.96843630740842,-2.24978152620299,-0.709398069659118));
#35048=CARTESIAN_POINT('Ctrl Pts',(2.09565514259353,-0.620502089064916,
-2.27590338356333));
#35049=CARTESIAN_POINT('Ctrl Pts',(2.22287397777864,1.57839809730298,-1.75311364786995));
#35050=CARTESIAN_POINT('Ctrl Pts',(2.35009281296375,2.32832610584676,0.379041259626889));
#35051=CARTESIAN_POINT('Ctrl Pts',(2.47731164814887,0.940822490842265,2.16324281343369));
#35052=CARTESIAN_POINT('Ctrl Pts',(2.60453048333398,-1.31033627345084,1.96155629457787));
#35053=CARTESIAN_POINT('Ctrl Pts',(2.73174931851909,-2.35864750248118,-0.0408174849469316));
#35054=CARTESIAN_POINT('Ctrl Pts',(2.85896815370421,-1.24161073233134,-2.00578545294822));
#35055=CARTESIAN_POINT('Ctrl Pts',(2.98618698888932,1.01505102673121,-2.12930526437765));
#35056=CARTESIAN_POINT('Ctrl Pts',(3.11340582407443,2.34023742749476,-0.298347997134086));
#35057=CARTESIAN_POINT('Ctrl Pts',(3.24062465925955,1.51640407537933,1.80695219210931));
#35058=CARTESIAN_POINT('Ctrl Pts',(3.36784349444466,-0.698217180620254,
2.25257951257453));
#35059=CARTESIAN_POINT('Ctrl Pts',(3.49506232962978,-2.27434460912666,0.632031074066706));
#35060=CARTESIAN_POINT('Ctrl Pts',(3.62228116481489,-1.7576911784917,-1.57218661975746));
#35061=CARTESIAN_POINT('Ctrl Pts',(3.70709372160496,-0.344875555534673,
-2.07399924429869));
#35062=CARTESIAN_POINT('Ctrl Pts',(3.7495,0.311349471200418,-1.97030177112117));
#35063=CARTESIAN_POINT('Ctrl Pts',(0.275081743211219,-0.941790067967391,
1.92904360906014));
#35064=CARTESIAN_POINT('Ctrl Pts',(0.317488021606256,-1.58427372832989,
1.61537276858829));
#35065=CARTESIAN_POINT('Ctrl Pts',(0.402300578396332,-2.51992744547999,
0.300899277314577));
#35066=CARTESIAN_POINT('Ctrl Pts',(0.529519413581445,-1.61472172164465,
-1.96107696748283));
#35067=CARTESIAN_POINT('Ctrl Pts',(0.656738248766559,0.775007876324146,
-2.41668555342406));
#35068=CARTESIAN_POINT('Ctrl Pts',(0.783957083951671,2.45214790396061,-0.656792957612989));
#35069=CARTESIAN_POINT('Ctrl Pts',(0.911175919136786,1.8787867383313,1.70760538808775));
#35070=CARTESIAN_POINT('Ctrl Pts',(1.0383947543219,-0.419618044214592,2.50359610064302));
#35071=CARTESIAN_POINT('Ctrl Pts',(1.16561358950701,-2.33265142423783,1.00169486454339));
#35072=CARTESIAN_POINT('Ctrl Pts',(1.29283242469213,-2.1043792464395,-1.41999032320318));
#35073=CARTESIAN_POINT('Ctrl Pts',(1.42005125987724,0.055769785018477,-2.53799976334616));
#35074=CARTESIAN_POINT('Ctrl Pts',(1.54727009506235,2.16469908833949,-1.3261697108228));
#35075=CARTESIAN_POINT('Ctrl Pts',(1.67448893024746,2.2864329274227,1.10312389541923));
#35076=CARTESIAN_POINT('Ctrl Pts',(1.80170776543258,0.309200455317831,2.51972657221502));
#35077=CARTESIAN_POINT('Ctrl Pts',(1.92892660061769,-1.95187621229853,1.62321254164996));
#35078=CARTESIAN_POINT('Ctrl Pts',(2.0561454358028,-2.42112094727782,-0.763424584301242));
#35079=CARTESIAN_POINT('Ctrl Pts',(2.18336427098792,-0.667758441505294,
-2.44923219954846));
#35080=CARTESIAN_POINT('Ctrl Pts',(2.31058310617303,1.69860613220222,-1.88662771312737));
#35081=CARTESIAN_POINT('Ctrl Pts',(2.43780194135814,2.50564734455498,0.407908378158857));
#35082=CARTESIAN_POINT('Ctrl Pts',(2.56502077654326,1.0124738841165,2.32799159769612));
#35083=CARTESIAN_POINT('Ctrl Pts',(2.69223961172837,-1.41012918929246,2.11094498677051));
#35084=CARTESIAN_POINT('Ctrl Pts',(2.81945844691349,-2.53827796565631,-0.0439260731183047));
#35085=CARTESIAN_POINT('Ctrl Pts',(2.9466772820986,-1.33616963131785,-2.15854256038544));
#35086=CARTESIAN_POINT('Ctrl Pts',(3.07389611728371,1.09235553530501,-2.29146942433756));
#35087=CARTESIAN_POINT('Ctrl Pts',(3.20111495246883,2.51846581159982,-0.321069658109792));
#35088=CARTESIAN_POINT('Ctrl Pts',(3.32833378765394,1.63189075413675,1.94456650661051));
#35089=CARTESIAN_POINT('Ctrl Pts',(3.45555262283905,-0.751392178333865,
2.4241320233914));
#35090=CARTESIAN_POINT('Ctrl Pts',(3.58277145802416,-2.44755471158052,0.680165453814528));
#35091=CARTESIAN_POINT('Ctrl Pts',(3.70999029320928,-1.89155386046481,-1.69192159940477));
#35092=CARTESIAN_POINT('Ctrl Pts',(3.79480284999935,-0.371140673876142,
-2.23195139462481));
#35093=CARTESIAN_POINT('Ctrl Pts',(3.83720912839439,0.335061301672003,-2.12035650349172));
#35094=CARTESIAN_POINT('Ctrl Pts',(0.362790871605609,-1.00843926415934,
2.06555938931311));
#35095=CARTESIAN_POINT('Ctrl Pts',(0.405197150000647,-1.6963906152377,1.72969049207961));
#35096=CARTESIAN_POINT('Ctrl Pts',(0.490009706790723,-2.69825926741749,
0.322193508003416));
#35097=CARTESIAN_POINT('Ctrl Pts',(0.617228541975836,-1.7289933714334,-2.09985970473909));
#35098=CARTESIAN_POINT('Ctrl Pts',(0.744447377160949,0.82985412471463,-2.58771108773664));
#35099=CARTESIAN_POINT('Ctrl Pts',(0.871666212346062,2.62568306036279,-0.7032732977422));
#35100=CARTESIAN_POINT('Ctrl Pts',(0.998885047531176,2.01174590851678,1.82845028802889));
#35101=CARTESIAN_POINT('Ctrl Pts',(1.12610388271629,-0.449313839812542,
2.68077217562253));
#35102=CARTESIAN_POINT('Ctrl Pts',(1.2533227179014,-2.49772997805715,1.07258344133154));
#35103=CARTESIAN_POINT('Ctrl Pts',(1.38054155308652,-2.25330329016074,-1.52048109801682));
#35104=CARTESIAN_POINT('Ctrl Pts',(1.50776038827163,0.0597165364970737,
-2.71761053852396));
#35105=CARTESIAN_POINT('Ctrl Pts',(1.63497922345674,2.31789188484737,-1.42002092910036));
#35106=CARTESIAN_POINT('Ctrl Pts',(1.76219805864185,2.44824066137811,1.18119046612379));
#35107=CARTESIAN_POINT('Ctrl Pts',(1.88941689382697,0.331082149030738,2.69804417862604));
#35108=CARTESIAN_POINT('Ctrl Pts',(2.01663572901208,-2.09000782468285,1.73808507516812));
#35109=CARTESIAN_POINT('Ctrl Pts',(2.14385456419719,-2.59246036835264,-0.817451098943368));
#35110=CARTESIAN_POINT('Ctrl Pts',(2.27107339938231,-0.715014793945677,
-2.62256101553358));
#35111=CARTESIAN_POINT('Ctrl Pts',(2.39829223456742,1.81881416710148,-2.02014177838479));
#35112=CARTESIAN_POINT('Ctrl Pts',(2.52551106975254,2.6829685832632,0.436775496690829));
#35113=CARTESIAN_POINT('Ctrl Pts',(2.65272990493765,1.08412527739075,2.49274038195854));
#35114=CARTESIAN_POINT('Ctrl Pts',(2.77994874012277,-1.50992210513408,2.26033367896316));
#35115=CARTESIAN_POINT('Ctrl Pts',(2.90716757530787,-2.71790842883145,-0.0470346612896804));
#35116=CARTESIAN_POINT('Ctrl Pts',(3.03438641049299,-1.43072853030436,-2.31129966782265));
#35117=CARTESIAN_POINT('Ctrl Pts',(3.1616052456781,1.1696600438788,-2.45363358429747));
#35118=CARTESIAN_POINT('Ctrl Pts',(3.28882408086321,2.69669419570489,-0.343791319085499));
#35119=CARTESIAN_POINT('Ctrl Pts',(3.41604291604833,1.74737743289418,2.08218082111171));
#35120=CARTESIAN_POINT('Ctrl Pts',(3.54326175123344,-0.804567176047475,
2.59568453420827));
#35121=CARTESIAN_POINT('Ctrl Pts',(3.67048058641855,-2.62076481403437,0.72829983356235));
#35122=CARTESIAN_POINT('Ctrl Pts',(3.79769942160367,-2.02541654243792,-1.81165657905209));
#35123=CARTESIAN_POINT('Ctrl Pts',(3.88251197839374,-0.39740579221761,-2.38990354495094));
#35124=CARTESIAN_POINT('Ctrl Pts',(3.92491825678878,0.358773132143588,-2.27041123586227));
#35125=CARTESIAN_POINT('Ctrl Pts',(0.4505,-1.07508846035128,2.20207516956609));
#35126=CARTESIAN_POINT('Ctrl Pts',(0.492906278395038,-1.80850750214552,
1.84400821557094));
#35127=CARTESIAN_POINT('Ctrl Pts',(0.577718835185112,-2.87659108935499,
0.343487738692257));
#35128=CARTESIAN_POINT('Ctrl Pts',(0.704937670370228,-1.84326502122216,
-2.23864244199535));
#35129=CARTESIAN_POINT('Ctrl Pts',(0.832156505555339,0.884700373105116,
-2.75873662204922));
#35130=CARTESIAN_POINT('Ctrl Pts',(0.959375340740454,2.79921821676497,-0.749753637871415));
#35131=CARTESIAN_POINT('Ctrl Pts',(1.08659417592557,2.14470507870227,1.94929518797004));
#35132=CARTESIAN_POINT('Ctrl Pts',(1.21381301111068,-0.479009635410491,
2.85794825060204));
#35133=CARTESIAN_POINT('Ctrl Pts',(1.34103184629579,-2.66280853187646,1.14347201811968));
#35134=CARTESIAN_POINT('Ctrl Pts',(1.46825068148091,-2.40222733388198,-1.62097187283046));
#35135=CARTESIAN_POINT('Ctrl Pts',(1.59546951666602,0.063663287975671,-2.89722131370176));
#35136=CARTESIAN_POINT('Ctrl Pts',(1.72268835185113,2.47108468135524,-1.51387214737792));
#35137=CARTESIAN_POINT('Ctrl Pts',(1.84990718703624,2.61004839533353,1.25925703682834));
#35138=CARTESIAN_POINT('Ctrl Pts',(1.97712602222136,0.352963842743642,2.87636178503707));
#35139=CARTESIAN_POINT('Ctrl Pts',(2.10434485740647,-2.22813943706718,1.85295760868628));
#35140=CARTESIAN_POINT('Ctrl Pts',(2.23156369259159,-2.76379978942746,-0.871477613585491));
#35141=CARTESIAN_POINT('Ctrl Pts',(2.3587825277767,-0.762271146386054,-2.79588983151871));
#35142=CARTESIAN_POINT('Ctrl Pts',(2.48600136296182,1.93902220200072,-2.15365584364221));
#35143=CARTESIAN_POINT('Ctrl Pts',(2.61322019814693,2.86028982197142,0.4656426152228));
#35144=CARTESIAN_POINT('Ctrl Pts',(2.74043903333204,1.15577667066498,2.65748916622096));
#35145=CARTESIAN_POINT('Ctrl Pts',(2.86765786851715,-1.60971502097569,2.40972237115582));
#35146=CARTESIAN_POINT('Ctrl Pts',(2.99487670370227,-2.89753889200658,-0.050143249461057));
#35147=CARTESIAN_POINT('Ctrl Pts',(3.12209553888738,-1.52528742929087,-2.46405677525986));
#35148=CARTESIAN_POINT('Ctrl Pts',(3.2493143740725,1.2469645524526,-2.61579774425739));
#35149=CARTESIAN_POINT('Ctrl Pts',(3.3765332092576,2.87492257980995,-0.366512980061205));
#35150=CARTESIAN_POINT('Ctrl Pts',(3.50375204444272,1.86286411165161,2.21979513561292));
#35151=CARTESIAN_POINT('Ctrl Pts',(3.63097087962783,-0.857742173761087,
2.76723704502514));
#35152=CARTESIAN_POINT('Ctrl Pts',(3.75818971481295,-2.79397491648822,0.776434213310176));
#35153=CARTESIAN_POINT('Ctrl Pts',(3.88540854999806,-2.15927922441104,-1.93139155869941));
#35154=CARTESIAN_POINT('Ctrl Pts',(3.97022110678813,-0.423670910559079,
-2.54785569527707));
#35155=CARTESIAN_POINT('Ctrl Pts',(4.01262738518317,0.382484962615173,-2.42046596823283));
#35156=CARTESIAN_POINT('Ctrl Pts',(2.99267250378795,-2.45452615968528,-0.000257956296186217));
#35157=CARTESIAN_POINT('Ctrl Pts',(2.99340723709272,-2.45454751304904,-0.0143344873317633));
#35158=CARTESIAN_POINT('Ctrl Pts',(2.99414197039749,-2.45443680249629,-0.0284106766992283));
#35159=CARTESIAN_POINT('Ctrl Pts',(2.99487670370227,-2.45419300304882,-0.0424845669913881));
#35160=CARTESIAN_POINT('Ctrl Pts',(3.0372829820973,-2.44012173776801,-0.854781091393998));
#35161=CARTESIAN_POINT('Ctrl Pts',(3.07968926049234,-1.98270458352944,-1.65941893332693));
#35162=CARTESIAN_POINT('Ctrl Pts',(3.12209553888738,-1.29195400945291,-2.08702801579298));
#35163=CARTESIAN_POINT('Ctrl Pts',(3.16450181728242,-0.601203435376382,
-2.51463709825904));
#35164=CARTESIAN_POINT('Ctrl Pts',(3.20690809567746,0.322880558538104,-2.56521742125821));
#35165=CARTESIAN_POINT('Ctrl Pts',(3.24931437407249,1.05624889338824,-2.21562678872511));
#35166=CARTESIAN_POINT('Ctrl Pts',(3.29172065246753,1.78961722823838,-1.866036156192));
#35167=CARTESIAN_POINT('Ctrl Pts',(3.33412693086257,2.33226990402417,-1.1162745681266));
#35168=CARTESIAN_POINT('Ctrl Pts',(3.37653320925761,2.43491983055733,-0.310342421481551));
#35169=CARTESIAN_POINT('Ctrl Pts',(3.41893948765264,2.5375697570905,0.495589725163502));
#35170=CARTESIAN_POINT('Ctrl Pts',(3.46134576604768,2.20021693437105,1.35769243038821));
#35171=CARTESIAN_POINT('Ctrl Pts',(3.50375204444272,1.57810614210921,1.87998410123594));
#35172=CARTESIAN_POINT('Ctrl Pts',(3.54615832283776,0.955995349847373,2.40227577208366));
#35173=CARTESIAN_POINT('Ctrl Pts',(3.58856460123279,0.0491265880431435,
2.5847564085544));
#35174=CARTESIAN_POINT('Ctrl Pts',(3.63097087962783,-0.727013249980161,
2.34419625483728));
#35175=CARTESIAN_POINT('Ctrl Pts',(3.67048058641855,-1.45013865945934,2.1200676234503));
#35176=CARTESIAN_POINT('Ctrl Pts',(3.70999029320928,-2.05978415989638,1.52871627651428));
#35177=CARTESIAN_POINT('Ctrl Pts',(3.7495,-2.31513335459632,0.815631492636623));
#35178=CARTESIAN_POINT('',(0.4505,-1.16034898466907,-1.62253437445173));
#35179=CARTESIAN_POINT('Ctrl Pts',(0.450499999999999,-1.16286240980301,
-1.62484720205836));
#35180=CARTESIAN_POINT('Ctrl Pts',(0.450499999999999,-1.20286330961462,
-1.60271479777366));
#35181=CARTESIAN_POINT('Ctrl Pts',(0.450499999999999,-1.24197977006801,
-1.579152801667));
#35182=CARTESIAN_POINT('Ctrl Pts',(0.450499999999999,-1.28012567116714,
-1.55417759699536));
#35183=CARTESIAN_POINT('Ctrl Pts',(0.4505,-1.34003952566005,-1.5149502950963));
#35184=CARTESIAN_POINT('Ctrl Pts',(0.4505,-1.39756042503822,-1.47223942604334));
#35185=CARTESIAN_POINT('Ctrl Pts',(0.4505,-1.45260638718602,-1.42638958840563));
#35186=CARTESIAN_POINT('Ctrl Pts',(0.450499999999999,-1.48312159761652,
-1.40097233000688));
#35187=CARTESIAN_POINT('Ctrl Pts',(0.4505,-1.51287592931269,-1.37458951272792));
#35188=CARTESIAN_POINT('Ctrl Pts',(0.4505,-1.54185269550254,-1.34729371270681));
#35189=CARTESIAN_POINT('Ctrl Pts',(0.4505,-1.55613672552596,-1.3338383110771));
#35190=CARTESIAN_POINT('Ctrl Pts',(0.4505,-1.57023177572244,-1.32016099482662));
#35191=CARTESIAN_POINT('Ctrl Pts',(0.4505,-1.58413563760341,-1.30626771878357));
#35192=CARTESIAN_POINT('Ctrl Pts',(0.4505,-1.59424325015721,-1.29616780175704));
#35193=CARTESIAN_POINT('Ctrl Pts',(0.4505,-1.60424293841027,-1.2859606250128));
#35194=CARTESIAN_POINT('Ctrl Pts',(0.4505,-1.61413396809427,-1.27564913736583));
#35195=CARTESIAN_POINT('Ctrl Pts',(0.4505,-1.66618304361349,-1.22138750673695));
#35196=CARTESIAN_POINT('Ctrl Pts',(0.4505,-1.71522672419473,-1.16423977664219));
#35197=CARTESIAN_POINT('Ctrl Pts',(0.4505,-1.76117091050649,-1.10457870598492));
#35198=CARTESIAN_POINT('Ctrl Pts',(0.4505,-1.79851739430398,-1.05608222824728));
#35199=CARTESIAN_POINT('Ctrl Pts',(0.4505,-1.83381563167038,-1.00592385645458));
#35200=CARTESIAN_POINT('Ctrl Pts',(0.4505,-1.86700175841926,-0.954282216791985));
#35201=CARTESIAN_POINT('Ctrl Pts',(0.4505,-1.8801338745443,-0.933847050794197));
#35202=CARTESIAN_POINT('Ctrl Pts',(0.4505,-1.8929351120508,-0.913179436076022));
#35203=CARTESIAN_POINT('Ctrl Pts',(0.4505,-1.90540088753822,-0.892289759695898));
#35204=CARTESIAN_POINT('Ctrl Pts',(0.4505,-1.91424907112747,-0.877462307371091));
#35205=CARTESIAN_POINT('Ctrl Pts',(0.4505,-1.92292961817841,-0.86252027332416));
#35206=CARTESIAN_POINT('Ctrl Pts',(0.4505,-1.93142873757601,-0.847489309628046));
#35207=CARTESIAN_POINT('Ctrl Pts',(0.4505,-1.96971919482744,-0.779771414875745));
#35208=CARTESIAN_POINT('Ctrl Pts',(0.4505,-2.00438315634146,-0.710165083960324));
#35209=CARTESIAN_POINT('Ctrl Pts',(0.4505,-2.0353241077575,-0.639048694689319));
#35210=CARTESIAN_POINT('Ctrl Pts',(0.4505,-2.06685107805879,-0.566585367290814));
#35211=CARTESIAN_POINT('Ctrl Pts',(0.4505,-2.09451336057944,-0.49255347892645));
#35212=CARTESIAN_POINT('Ctrl Pts',(0.4505,-2.11817370236006,-0.417312725162707));
#35213=CARTESIAN_POINT('Ctrl Pts',(0.4505,-2.13546259495292,-0.362333413262279));
#35214=CARTESIAN_POINT('Ctrl Pts',(0.4505,-2.15061399663607,-0.30670773008184));
#35215=CARTESIAN_POINT('Ctrl Pts',(0.4505,-2.16355960203642,-0.250566432797886));
#35216=CARTESIAN_POINT('Ctrl Pts',(0.4505,-2.17326880608668,-0.20846045983492));
#35217=CARTESIAN_POINT('Ctrl Pts',(0.4505,-2.18173700276312,-0.1660642755761));
#35218=CARTESIAN_POINT('Ctrl Pts',(0.4505,-2.18893003555588,-0.123431179597991));
#35219=CARTESIAN_POINT('Ctrl Pts',(0.4505,-2.19111103153329,-0.110504419285397));
#35220=CARTESIAN_POINT('Ctrl Pts',(0.4505,-2.19317506525113,-0.0975538196791666));
#35221=CARTESIAN_POINT('Ctrl Pts',(0.4505,-2.19512011992499,-0.0845873892082416));
#35222=CARTESIAN_POINT('Ctrl Pts',(0.4505,-2.2071501360141,-0.00439099715827403));
#35223=CARTESIAN_POINT('Ctrl Pts',(0.4505,-2.21459346758939,0.0761401520900184));
#35224=CARTESIAN_POINT('Ctrl Pts',(0.4505,-2.21732325800404,0.15662739588242));
#35225=CARTESIAN_POINT('Ctrl Pts',(0.4505,-2.2185190065568,0.191883767494183));
#35226=CARTESIAN_POINT('Ctrl Pts',(0.4505,-2.21880979474632,0.227132116865632));
#35227=CARTESIAN_POINT('Ctrl Pts',(0.4505,-2.21818221942756,0.262342172420224));
#35228=CARTESIAN_POINT('Ctrl Pts',(0.4505,-2.21679935655232,0.339927566884592));
#35229=CARTESIAN_POINT('Ctrl Pts',(0.4505,-2.21096111363732,0.41732659146968));
#35230=CARTESIAN_POINT('Ctrl Pts',(0.4505,-2.20090098242755,0.49428846405244));
#35231=CARTESIAN_POINT('Ctrl Pts',(0.4505,-2.19063003840118,0.572863093843948));
#35232=CARTESIAN_POINT('Ctrl Pts',(0.4505,-2.17595829487236,0.65098282970126));
#35233=CARTESIAN_POINT('Ctrl Pts',(0.4505,-2.15708029963991,0.728383125138283));
#35234=CARTESIAN_POINT('Ctrl Pts',(0.4505,-2.15396392646031,0.741160340188063));
#35235=CARTESIAN_POINT('Ctrl Pts',(0.4505,-2.15073281306651,0.753917939175734));
#35236=CARTESIAN_POINT('Ctrl Pts',(0.4505,-2.14738770094255,0.766654714405889));
#35237=CARTESIAN_POINT('Ctrl Pts',(0.4505,-2.1442095939825,0.778755604453134));
#35238=CARTESIAN_POINT('Ctrl Pts',(0.4505,-2.14093109831446,0.790828124513886));
#35239=CARTESIAN_POINT('Ctrl Pts',(0.4505,-2.13755345581554,0.802870818443932));
#35240=CARTESIAN_POINT('Ctrl Pts',(0.4505,-2.11567321858042,0.880882923106774));
#35241=CARTESIAN_POINT('Ctrl Pts',(0.4505,-2.0896352327598,0.957648854289395));
#35242=CARTESIAN_POINT('Ctrl Pts',(0.4505,-2.05971373326038,1.03289773290721));
#35243=CARTESIAN_POINT('Ctrl Pts',(0.4505,-2.02920890208329,1.10961361870521));
#35244=CARTESIAN_POINT('Ctrl Pts',(0.4505,-1.99466746728849,1.18475355617105));
#35245=CARTESIAN_POINT('Ctrl Pts',(0.4505,-1.95632475170503,1.25803177794143));
#35246=CARTESIAN_POINT('Ctrl Pts',(0.4505,-1.91771233699759,1.33182543196321));
#35247=CARTESIAN_POINT('Ctrl Pts',(0.4505,-1.8752446472627,1.40373200500635));
#35248=CARTESIAN_POINT('Ctrl Pts',(0.4505,-1.8291106405353,1.47344764264672));
#35249=CARTESIAN_POINT('Ctrl Pts',(0.4505,-1.81079706334026,1.50112229746639));
#35250=CARTESIAN_POINT('Ctrl Pts',(0.4505,-1.79190520610228,1.52845149410343));
#35251=CARTESIAN_POINT('Ctrl Pts',(0.4505,-1.77244484874189,1.55541520292446));
#35252=CARTESIAN_POINT('Ctrl Pts',(0.4505,-1.76269243849393,1.56892786075285));
#35253=CARTESIAN_POINT('Ctrl Pts',(0.4505,-1.75279510256798,1.58235137285538));
#35254=CARTESIAN_POINT('Ctrl Pts',(0.4505,-1.74276980623577,1.59566264979496));
#35255=CARTESIAN_POINT('Ctrl Pts',(0.4505,-1.69110824500774,1.66425726544013));
#35256=CARTESIAN_POINT('Ctrl Pts',(0.4505,-1.63597635124539,1.72998168578403));
#35257=CARTESIAN_POINT('Ctrl Pts',(0.4505,-1.57763057533434,1.79253936164174));
#35258=CARTESIAN_POINT('Ctrl Pts',(0.4505,-1.51919556506657,1.85519271355955));
#35259=CARTESIAN_POINT('Ctrl Pts',(0.4505,-1.45753640083401,1.9146705632344));
#35260=CARTESIAN_POINT('Ctrl Pts',(0.4505,-1.39286151373016,1.9706576018754));
#35261=CARTESIAN_POINT('Ctrl Pts',(0.4505,-1.32955892208391,2.02545668701153));
#35262=CARTESIAN_POINT('Ctrl Pts',(0.4505,-1.26336666868825,2.07691231275167));
#35263=CARTESIAN_POINT('Ctrl Pts',(0.4505,-1.19444070240512,2.1246995984667));
#35264=CARTESIAN_POINT('Ctrl Pts',(0.4505,-1.15552113289993,2.15168305170129));
#35265=CARTESIAN_POINT('Ctrl Pts',(0.4505,-1.11572927824821,2.17749630300684));
#35266=CARTESIAN_POINT('Ctrl Pts',(0.4505,-1.07508846035128,2.20207516956609));
#35267=CARTESIAN_POINT('Ctrl Pts',(0.4505,-1.162862409803,-1.62484720205837));
#35268=CARTESIAN_POINT('Ctrl Pts',(0.490009706790723,-0.659641438489814,
-1.98109404025392));
#35269=CARTESIAN_POINT('Ctrl Pts',(0.571925691976483,0.755645094302849,
-2.20842574605865));
#35270=CARTESIAN_POINT('Ctrl Pts',(0.696247955557281,2.27861274755843,-0.610312617483778));
#35271=CARTESIAN_POINT('Ctrl Pts',(0.823466790742394,1.74582756814582,1.5867604881466));
#35272=CARTESIAN_POINT('Ctrl Pts',(0.950685625927508,-0.389922248616644,
2.3264200256635));
#35273=CARTESIAN_POINT('Ctrl Pts',(1.05271173521497,-1.81555058699103,1.20717506842332));
#35274=CARTESIAN_POINT('Ctrl Pts',(1.11233156610739,-1.99312914321941,0.271569088097866));
#35275=CARTESIAN_POINT('Ctrl Pts',(1.12954511860477,-1.99192664249562,0.000999255222959156));
#35276=CARTESIAN_POINT('Origin',(0.4505,-5.69858952725515E-16,8.58067791224701E-17));
#35277=CARTESIAN_POINT('',(0.4505,-2.4505,-3.00099698131059E-16));
#35278=CARTESIAN_POINT('Origin',(0.4505,0.,0.));
#35279=CARTESIAN_POINT('Origin',(0.4505,0.,0.));
#35280=CARTESIAN_POINT('',(0.4505,1.16034898466907,-1.62253437445173));
#35281=CARTESIAN_POINT('Ctrl Pts',(0.4505,1.07766119456972,2.20539011734829));
#35282=CARTESIAN_POINT('Ctrl Pts',(0.4505,1.1253722485115,2.17681124103074));
#35283=CARTESIAN_POINT('Ctrl Pts',(0.450499999999999,1.17197132590231,2.14653322621614));
#35284=CARTESIAN_POINT('Ctrl Pts',(0.450499999999999,1.21735566783477,2.11455018800921));
#35285=CARTESIAN_POINT('Ctrl Pts',(0.450499999999999,1.28700221983055,2.06546920019237));
#35286=CARTESIAN_POINT('Ctrl Pts',(0.4505,1.35379019187679,2.01237416511058));
#35287=CARTESIAN_POINT('Ctrl Pts',(0.4505,1.41755123156995,1.95562691189186));
#35288=CARTESIAN_POINT('Ctrl Pts',(0.4505,1.44984247863091,1.9268877385262));
#35289=CARTESIAN_POINT('Ctrl Pts',(0.450499999999999,1.48135671953801,1.89721129791422));
#35290=CARTESIAN_POINT('Ctrl Pts',(0.450499999999999,1.51206782367031,1.86664196767908));
#35291=CARTESIAN_POINT('Ctrl Pts',(0.450499999999999,1.53122947677371,1.8475687719045));
#35292=CARTESIAN_POINT('Ctrl Pts',(0.450499999999999,1.5500784167829,1.82814795145982));
#35293=CARTESIAN_POINT('Ctrl Pts',(0.450499999999999,1.56860768548358,1.80839005248937));
#35294=CARTESIAN_POINT('Ctrl Pts',(0.450499999999999,1.58037795787674,1.7958393222606));
#35295=CARTESIAN_POINT('Ctrl Pts',(0.450499999999999,1.59201302261345,1.78315914283905));
#35296=CARTESIAN_POINT('Ctrl Pts',(0.450499999999999,1.60350833805641,1.77035617908208));
#35297=CARTESIAN_POINT('Ctrl Pts',(0.450499999999999,1.660267874257,1.70713996823124));
#35298=CARTESIAN_POINT('Ctrl Pts',(0.4505,1.71365006389022,1.64090458616163));
#35299=CARTESIAN_POINT('Ctrl Pts',(0.4505,1.7634832017426,1.57200692669245));
#35300=CARTESIAN_POINT('Ctrl Pts',(0.4505,1.80175234668051,1.51909726397123));
#35301=CARTESIAN_POINT('Ctrl Pts',(0.450499999999999,1.83792764492218,1.46461675962789));
#35302=CARTESIAN_POINT('Ctrl Pts',(0.450499999999999,1.87191183530092,1.40871961920951));
#35303=CARTESIAN_POINT('Ctrl Pts',(0.450499999999999,1.88877785857892,1.38097841187271));
#35304=CARTESIAN_POINT('Ctrl Pts',(0.450499999999999,1.90510392941073,1.35288821271951));
#35305=CARTESIAN_POINT('Ctrl Pts',(0.450499999999999,1.92087647850637,1.32446762860519));
#35306=CARTESIAN_POINT('Ctrl Pts',(0.4505,1.9303350350449,1.30742423884786));
#35307=CARTESIAN_POINT('Ctrl Pts',(0.4505,1.93959678388073,1.29025743573171));
#35308=CARTESIAN_POINT('Ctrl Pts',(0.4505,1.94864464124469,1.27299863809729));
#35309=CARTESIAN_POINT('Ctrl Pts',(0.4505,1.98726093032314,1.19933802522641));
#35310=CARTESIAN_POINT('Ctrl Pts',(0.450499999999999,2.02203257416733,1.12392171655336));
#35311=CARTESIAN_POINT('Ctrl Pts',(0.450499999999999,2.05279909002309,1.04708127458096));
#35312=CARTESIAN_POINT('Ctrl Pts',(0.4505,2.08291604831929,0.971863125174856));
#35313=CARTESIAN_POINT('Ctrl Pts',(0.450499999999999,2.10919534613456,0.895279401798556));
#35314=CARTESIAN_POINT('Ctrl Pts',(0.450499999999999,2.13143843939754,0.817632103176601));
#35315=CARTESIAN_POINT('Ctrl Pts',(0.4505,2.15319308716667,0.74168989443012));
#35316=CARTESIAN_POINT('Ctrl Pts',(0.4505,2.17108694519009,0.664729532655734));
#35317=CARTESIAN_POINT('Ctrl Pts',(0.4505,2.18488617170524,0.587037321507561));
#35318=CARTESIAN_POINT('Ctrl Pts',(0.4505,2.18972785922178,0.559777720512106));
#35319=CARTESIAN_POINT('Ctrl Pts',(0.4505,2.19406502052564,0.532428111547084));
#35320=CARTESIAN_POINT('Ctrl Pts',(0.4505,2.19788607277123,0.505001239804802));
#35321=CARTESIAN_POINT('Ctrl Pts',(0.4505,2.20008575405405,0.489212296723147));
#35322=CARTESIAN_POINT('Ctrl Pts',(0.450499999999999,2.2021143818284,0.473397753261568));
#35323=CARTESIAN_POINT('Ctrl Pts',(0.450499999999999,2.2039696260404,0.457560083389685));
#35324=CARTESIAN_POINT('Ctrl Pts',(0.450499999999999,2.20542249242619,0.445157393739837));
#35325=CARTESIAN_POINT('Ctrl Pts',(0.4505,2.20676796699628,0.432749475626273));
#35326=CARTESIAN_POINT('Ctrl Pts',(0.4505,2.20800521290325,0.420339348883872));
#35327=CARTESIAN_POINT('Ctrl Pts',(0.4505,2.21574988769131,0.342656816125777));
#35328=CARTESIAN_POINT('Ctrl Pts',(0.4505,2.2192608461013,0.264863324756902));
#35329=CARTESIAN_POINT('Ctrl Pts',(0.4505,2.21835792731929,0.187237833426566));
#35330=CARTESIAN_POINT('Ctrl Pts',(0.4505,2.21805232660199,0.160964810531994));
#35331=CARTESIAN_POINT('Ctrl Pts',(0.4505,2.21724066358271,0.13471106740812));
#35332=CARTESIAN_POINT('Ctrl Pts',(0.4505,2.21591459644172,0.108487611054857));
#35333=CARTESIAN_POINT('Ctrl Pts',(0.4505,2.21191623246908,0.029418520298201));
#35334=CARTESIAN_POINT('Ctrl Pts',(0.4505,2.20324469891092,-0.0493767922785765));
#35335=CARTESIAN_POINT('Ctrl Pts',(0.4505,2.19008710614742,-0.127579539719568));
#35336=CARTESIAN_POINT('Ctrl Pts',(0.4505,2.17718423010061,-0.204268366839285));
#35337=CARTESIAN_POINT('Ctrl Pts',(0.450499999999999,2.15996657536957,-0.280388073854071));
#35338=CARTESIAN_POINT('Ctrl Pts',(0.450499999999999,2.13857057363323,-0.355611797093477));
#35339=CARTESIAN_POINT('Ctrl Pts',(0.450499999999999,2.13331188408938,-0.374100214309137));
#35340=CARTESIAN_POINT('Ctrl Pts',(0.4505,2.12779838008763,-0.392541028423528));
#35341=CARTESIAN_POINT('Ctrl Pts',(0.4505,2.12204347435241,-0.410893253784562));
#35342=CARTESIAN_POINT('Ctrl Pts',(0.4505,2.09876348753168,-0.485132447994281));
#35343=CARTESIAN_POINT('Ctrl Pts',(0.4505,2.0715155754429,-0.558010645131724));
#35344=CARTESIAN_POINT('Ctrl Pts',(0.4505,2.0405037686822,-0.629236342323922));
#35345=CARTESIAN_POINT('Ctrl Pts',(0.4505,2.00952043889923,-0.700396635632768));
#35346=CARTESIAN_POINT('Ctrl Pts',(0.4505,1.97477945052421,-0.769908288945355));
#35347=CARTESIAN_POINT('Ctrl Pts',(0.4505,1.93644161811572,-0.837451348638747));
#35348=CARTESIAN_POINT('Ctrl Pts',(0.4505,1.89874831846993,-0.903858879479057));
#35349=CARTESIAN_POINT('Ctrl Pts',(0.4505,1.85757740508633,-0.968364102521197));
#35350=CARTESIAN_POINT('Ctrl Pts',(0.4505,1.81305071976513,-1.0306238622284));
#35351=CARTESIAN_POINT('Ctrl Pts',(0.4505,1.79614454072544,-1.05426304931329));
#35352=CARTESIAN_POINT('Ctrl Pts',(0.4505,1.77875431794757,-1.07757806955031));
#35353=CARTESIAN_POINT('Ctrl Pts',(0.4505,1.76088583128245,-1.10054833472365));
#35354=CARTESIAN_POINT('Ctrl Pts',(0.4505,1.75326867502042,-1.11034032788372));
#35355=CARTESIAN_POINT('Ctrl Pts',(0.4505,1.74556442525531,-1.1200697467296));
#35356=CARTESIAN_POINT('Ctrl Pts',(0.4505,1.73778290495544,-1.12972366725519));
#35357=CARTESIAN_POINT('Ctrl Pts',(0.4505,1.69071713631285,-1.18811446653882));
#35358=CARTESIAN_POINT('Ctrl Pts',(0.4505,1.64074593468803,-1.24385231590744));
#35359=CARTESIAN_POINT('Ctrl Pts',(0.4505,1.58802192138046,-1.29665175191528));
#35360=CARTESIAN_POINT('Ctrl Pts',(0.4505,1.53615421651406,-1.34859365451648));
#35361=CARTESIAN_POINT('Ctrl Pts',(0.4505,1.48162173354821,-1.39769237127414));
#35362=CARTESIAN_POINT('Ctrl Pts',(0.4505,1.424543005305,-1.44363421728573));
#35363=CARTESIAN_POINT('Ctrl Pts',(0.4505,1.36929311706813,-1.4881040563249));
#35364=CARTESIAN_POINT('Ctrl Pts',(0.4505,1.31165695283869,-1.52961639546006));
#35365=CARTESIAN_POINT('Ctrl Pts',(0.4505,1.25172579891194,-1.56784107051692));
#35366=CARTESIAN_POINT('Ctrl Pts',(0.4505,1.22183450271092,-1.58690603104995));
#35367=CARTESIAN_POINT('Ctrl Pts',(0.4505,1.19137209683489,-1.60515239365456));
#35368=CARTESIAN_POINT('Ctrl Pts',(0.4505,1.16034898466907,-1.62253437445173));
#35369=CARTESIAN_POINT('Origin',(0.4505,0.,0.));
#35370=CARTESIAN_POINT('Origin',(-1.02854511860477,0.,0.));
#35371=CARTESIAN_POINT('Ctrl Pts',(0.4505,1.16034898466907,-1.62253437445173));
#35372=CARTESIAN_POINT('Ctrl Pts',(0.492906278395038,1.70074725201027,-1.23607070952126));
#35373=CARTESIAN_POINT('Ctrl Pts',(0.577718835185113,2.35553983219541,0.112669531194497));
#35374=CARTESIAN_POINT('Ctrl Pts',(0.704937670370226,1.17739386665123,2.04593681646151));
#35375=CARTESIAN_POINT('Ctrl Pts',(0.83215650555534,-1.0826777789212,2.09509384907487));
#35376=CARTESIAN_POINT('Ctrl Pts',(0.920995575897006,-1.96647049832517,
0.78840734607953));
#35377=CARTESIAN_POINT('Ctrl Pts',(0.967428367843636,-1.99769546358392,
0.0640753932799172));
#35378=CARTESIAN_POINT('Ctrl Pts',(0.971454881395227,-1.99728088898927,
0.00122486924751962));
#35379=CARTESIAN_POINT('Ctrl Pts',(0.187372614816828,1.42545942445497,-1.99324250386964));
#35380=CARTESIAN_POINT('Ctrl Pts',(0.229778893211866,2.08932504877863,-1.51848165117526));
#35381=CARTESIAN_POINT('Ctrl Pts',(0.314591450001941,2.89372119754097,0.138411673739624));
#35382=CARTESIAN_POINT('Ctrl Pts',(0.441810285187055,1.44639863152217,2.51338171136179));
#35383=CARTESIAN_POINT('Ctrl Pts',(0.569029120372167,-1.33004230968612,
2.57376988452587));
#35384=CARTESIAN_POINT('Ctrl Pts',(0.696247955557282,-2.88480482818958,
0.275055317538262));
#35385=CARTESIAN_POINT('Ctrl Pts',(0.823466790742394,-1.79165965660462,
-2.27804038996095));
#35386=CARTESIAN_POINT('Ctrl Pts',(0.950685625927509,0.946429080626742,
-2.73890203154562));
#35387=CARTESIAN_POINT('Ctrl Pts',(1.07790446111262,2.81559143218447,-0.685944933469733));
#35388=CARTESIAN_POINT('Ctrl Pts',(1.20512329629773,2.10007452551338,1.99698045214554));
#35389=CARTESIAN_POINT('Ctrl Pts',(1.33234213148285,-0.54335094423318,2.84652607934227));
#35390=CARTESIAN_POINT('Ctrl Pts',(1.45956096666796,-2.68796270560187,1.08301537658065));
#35391=CARTESIAN_POINT('Ctrl Pts',(1.58677980185308,-2.36501524531905,-1.67474809746095));
#35392=CARTESIAN_POINT('Ctrl Pts',(1.71399863703819,0.129035324547271,-2.89506263077516));
#35393=CARTESIAN_POINT('Ctrl Pts',(1.8412174722233,2.50462795093246,-1.45770139723891));
#35394=CARTESIAN_POINT('Ctrl Pts',(1.96843630740841,2.58095870736468,1.31784367962883));
#35395=CARTESIAN_POINT('Ctrl Pts',(2.09565514259353,0.287949939112121,2.88359833691687));
#35396=CARTESIAN_POINT('Ctrl Pts',(2.22287397777864,-2.26939342905054,1.80219067117606));
#35397=CARTESIAN_POINT('Ctrl Pts',(2.35009281296376,-2.74342899054083,-0.933635728965404));
#35398=CARTESIAN_POINT('Ctrl Pts',(2.47731164814887,-0.698961077714174,
-2.81238674873448));
#35399=CARTESIAN_POINT('Ctrl Pts',(2.60453048333398,1.98712247865483,-2.10933288596168));
#35400=CARTESIAN_POINT('Ctrl Pts',(2.73174931851909,2.84908212195303,0.530070751248655));
#35401=CARTESIAN_POINT('Ctrl Pts',(2.85896815370421,1.09543795124656,2.68292587667123));
#35402=CARTESIAN_POINT('Ctrl Pts',(2.98618698888932,-1.6635791259226,2.3727235057746));
#35403=CARTESIAN_POINT('Ctrl Pts',(3.11340582407443,-2.89589144198292,-0.115434395429308));
#35404=CARTESIAN_POINT('Ctrl Pts',(3.24062465925955,-1.46885379292453,-2.49804380655408));
#35405=CARTESIAN_POINT('Ctrl Pts',(3.36784349444466,1.30486728963842,-2.58662430988328));
#35406=CARTESIAN_POINT('Ctrl Pts',(3.49506232962977,2.88406110179725,-0.302238629855752));
#35407=CARTESIAN_POINT('Ctrl Pts',(3.62228116481489,1.8089990872024,2.26280853432768));
#35408=CARTESIAN_POINT('Ctrl Pts',(3.70709372160496,-0.00481760480854868,
2.58283613012782));
#35409=CARTESIAN_POINT('Ctrl Pts',(3.7495,-0.778675485261984,2.32349192782157));
#35410=CARTESIAN_POINT('Ctrl Pts',(0.275081743211218,1.33708927785967,-1.869673127397));
#35411=CARTESIAN_POINT('Ctrl Pts',(0.317488021606256,1.95979911652251,-1.42434467062392));
#35412=CARTESIAN_POINT('Ctrl Pts',(0.402300578396332,2.71432740909245,0.129830959557915));
#35413=CARTESIAN_POINT('Ctrl Pts',(0.529519413581445,1.35673037656519,2.35756674639503));
#35414=CARTESIAN_POINT('Ctrl Pts',(0.656738248766558,-1.24758746609781,
2.4142112060422));
#35415=CARTESIAN_POINT('Ctrl Pts',(0.783957083951673,-2.7059638024877,0.258003496689719));
#35416=CARTESIAN_POINT('Ctrl Pts',(0.911175919136785,-1.68058723757483,
-2.13681521037519));
#35417=CARTESIAN_POINT('Ctrl Pts',(1.0383947543219,0.887756013430166,-2.56910612582884));
#35418=CARTESIAN_POINT('Ctrl Pts',(1.16561358950701,2.64104123219561,-0.643420359786968));
#35419=CARTESIAN_POINT('Ctrl Pts',(1.29283242469212,1.96988218857497,1.87317934474361));
#35420=CARTESIAN_POINT('Ctrl Pts',(1.42005125987724,-0.509666363829961,
2.67005811217091));
#35421=CARTESIAN_POINT('Ctrl Pts',(1.54727009506235,-2.52132474014202,1.01587475794817));
#35422=CARTESIAN_POINT('Ctrl Pts',(1.67448893024747,-2.21839813342976,-1.57092351126523));
#35423=CARTESIAN_POINT('Ctrl Pts',(1.80170776543258,0.12103588917185,-2.71558568131236));
#35424=CARTESIAN_POINT('Ctrl Pts',(1.92892660061769,2.34935566791029,-1.36733243691902));
#35425=CARTESIAN_POINT('Ctrl Pts',(2.05614543580281,2.42095436391349,1.2361450797525));
#35426=CARTESIAN_POINT('Ctrl Pts',(2.18336427098792,0.270098727148528,2.70483210661695));
#35427=CARTESIAN_POINT('Ctrl Pts',(2.31058310617303,-2.12870431046389,1.69046539084028));
#35428=CARTESIAN_POINT('Ctrl Pts',(2.43780194135815,-2.57335243984519,-0.875755774741645));
#35429=CARTESIAN_POINT('Ctrl Pts',(2.56502077654326,-0.655629579221588,
-2.63803522037486));
#35430=CARTESIAN_POINT('Ctrl Pts',(2.69223961172837,1.86393250794859,-1.97856658482899));
#35431=CARTESIAN_POINT('Ctrl Pts',(2.81945844691348,2.67245569509047,0.497209465132684));
#35432=CARTESIAN_POINT('Ctrl Pts',(2.9466772820986,1.02752720564626,2.51660016514394));
#35433=CARTESIAN_POINT('Ctrl Pts',(3.07389611728371,-1.56044695063331,2.22562852682381));
#35434=CARTESIAN_POINT('Ctrl Pts',(3.20111495246883,-2.71636311107307,-0.108278138105376));
#35435=CARTESIAN_POINT('Ctrl Pts',(3.32833378765393,-1.37779344930413,-2.34317970197175));
#35436=CARTESIAN_POINT('Ctrl Pts',(3.45555262283906,1.22397315004069,-2.42626873221488));
#35437=CARTESIAN_POINT('Ctrl Pts',(3.58277145802416,2.70526618278153,-0.283501602642697));
#35438=CARTESIAN_POINT('Ctrl Pts',(3.70999029320928,1.69685172489641,2.12252764069783));
#35439=CARTESIAN_POINT('Ctrl Pts',(3.79480284999935,-0.00451894148929613,
2.42271539744663));
#35440=CARTESIAN_POINT('Ctrl Pts',(3.83720912839439,-0.730402159762679,
2.17944901874116));
#35441=CARTESIAN_POINT('Ctrl Pts',(0.362790871605609,1.24871913126437,-1.74610375092437));
#35442=CARTESIAN_POINT('Ctrl Pts',(0.405197150000647,1.83027318426639,-1.33020769007259));
#35443=CARTESIAN_POINT('Ctrl Pts',(0.490009706790722,2.53493362064393,0.121250245376206));
#35444=CARTESIAN_POINT('Ctrl Pts',(0.617228541975837,1.26706212160821,2.20175178142827));
#35445=CARTESIAN_POINT('Ctrl Pts',(0.744447377160948,-1.1651326225095,2.25465252755853));
#35446=CARTESIAN_POINT('Ctrl Pts',(0.871666212346063,-2.52712277678581,
0.240951675841176));
#35447=CARTESIAN_POINT('Ctrl Pts',(0.998885047531177,-1.56951481854503,
-1.99559003078943));
#35448=CARTESIAN_POINT('Ctrl Pts',(1.12610388271629,0.829082946233588,-2.39931022011206));
#35449=CARTESIAN_POINT('Ctrl Pts',(1.2533227179014,2.46649103220676,-0.600895786104207));
#35450=CARTESIAN_POINT('Ctrl Pts',(1.38054155308651,1.83968985163656,1.74937823734167));
#35451=CARTESIAN_POINT('Ctrl Pts',(1.50776038827163,-0.475981783426744,
2.49359014499956));
#35452=CARTESIAN_POINT('Ctrl Pts',(1.63497922345674,-2.35468677468218,0.948734139315698));
#35453=CARTESIAN_POINT('Ctrl Pts',(1.76219805864186,-2.07178102154046,-1.46709892506951));
#35454=CARTESIAN_POINT('Ctrl Pts',(1.88941689382697,0.113036453796428,-2.53610873184956));
#35455=CARTESIAN_POINT('Ctrl Pts',(2.01663572901208,2.19408338488812,-1.27696347659914));
#35456=CARTESIAN_POINT('Ctrl Pts',(2.14385456419719,2.26095002046229,1.15444647987618));
#35457=CARTESIAN_POINT('Ctrl Pts',(2.27107339938231,0.252247515184935,2.52606587631703));
#35458=CARTESIAN_POINT('Ctrl Pts',(2.39829223456742,-1.98801519187724,1.5787401105045));
#35459=CARTESIAN_POINT('Ctrl Pts',(2.52551106975254,-2.40327588914955,-0.817875820517883));
#35460=CARTESIAN_POINT('Ctrl Pts',(2.65272990493765,-0.612298080729003,
-2.46368369201524));
#35461=CARTESIAN_POINT('Ctrl Pts',(2.77994874012277,1.74074253724235,-1.84780028369628));
#35462=CARTESIAN_POINT('Ctrl Pts',(2.90716757530787,2.49582926822791,0.464348179016712));
#35463=CARTESIAN_POINT('Ctrl Pts',(3.03438641049299,0.959616460045959,2.35027445361664));
#35464=CARTESIAN_POINT('Ctrl Pts',(3.1616052456781,-1.45731477534402,2.07853354787301));
#35465=CARTESIAN_POINT('Ctrl Pts',(3.28882408086321,-2.53683478016323,-0.101121880781441));
#35466=CARTESIAN_POINT('Ctrl Pts',(3.41604291604833,-1.28673310568374,-2.18831559738942));
#35467=CARTESIAN_POINT('Ctrl Pts',(3.54326175123344,1.14307901044296,-2.26591315454646));
#35468=CARTESIAN_POINT('Ctrl Pts',(3.67048058641856,2.5264712637658,-0.264764575429645));
#35469=CARTESIAN_POINT('Ctrl Pts',(3.79769942160367,1.58470436259042,1.98224674706799));
#35470=CARTESIAN_POINT('Ctrl Pts',(3.88251197839374,-0.00422027817004178,
2.26259466476544));
#35471=CARTESIAN_POINT('Ctrl Pts',(3.92491825678878,-0.682128834263374,
2.03540610966074));
#35472=CARTESIAN_POINT('Ctrl Pts',(0.4505,1.16034898466907,-1.62253437445173));
#35473=CARTESIAN_POINT('Ctrl Pts',(0.492906278395038,1.70074725201027,-1.23607070952126));
#35474=CARTESIAN_POINT('Ctrl Pts',(0.577718835185113,2.35553983219541,0.112669531194497));
#35475=CARTESIAN_POINT('Ctrl Pts',(0.704937670370226,1.17739386665123,2.04593681646151));
#35476=CARTESIAN_POINT('Ctrl Pts',(0.83215650555534,-1.0826777789212,2.09509384907487));
#35477=CARTESIAN_POINT('Ctrl Pts',(0.959375340740452,-2.34828175108393,
0.223899854992633));
#35478=CARTESIAN_POINT('Ctrl Pts',(1.08659417592557,-1.45844239951523,-1.85436485120368));
#35479=CARTESIAN_POINT('Ctrl Pts',(1.21381301111068,0.770409879037013,-2.22951431439528));
#35480=CARTESIAN_POINT('Ctrl Pts',(1.34103184629579,2.2919408322179,-0.558371212421443));
#35481=CARTESIAN_POINT('Ctrl Pts',(1.4682506814809,1.70949751469815,1.62557712993974));
#35482=CARTESIAN_POINT('Ctrl Pts',(1.59546951666602,-0.442297203023523,
2.3171221778282));
#35483=CARTESIAN_POINT('Ctrl Pts',(1.72268835185113,-2.18804880922234,0.881593520683224));
#35484=CARTESIAN_POINT('Ctrl Pts',(1.84990718703625,-1.92516390965116,-1.36327433887379));
#35485=CARTESIAN_POINT('Ctrl Pts',(1.97712602222136,0.105037018421004,-2.35663178238676));
#35486=CARTESIAN_POINT('Ctrl Pts',(2.10434485740647,2.03881110186596,-1.18659451627925));
#35487=CARTESIAN_POINT('Ctrl Pts',(2.23156369259159,2.1009456770111,1.07274787999985));
#35488=CARTESIAN_POINT('Ctrl Pts',(2.3587825277767,0.234396303221342,2.34729964601711));
#35489=CARTESIAN_POINT('Ctrl Pts',(2.48600136296182,-1.84732607329058,1.46701483016872));
#35490=CARTESIAN_POINT('Ctrl Pts',(2.61322019814693,-2.23319933845391,-0.759995866294124));
#35491=CARTESIAN_POINT('Ctrl Pts',(2.74043903333204,-0.568966582236417,
-2.28933216365562));
#35492=CARTESIAN_POINT('Ctrl Pts',(2.86765786851715,1.61755256653611,-1.71703398256359));
#35493=CARTESIAN_POINT('Ctrl Pts',(2.99487670370227,2.31920284136536,0.43148689290074));
#35494=CARTESIAN_POINT('Ctrl Pts',(3.12209553888738,0.891705714445654,2.18394874208935));
#35495=CARTESIAN_POINT('Ctrl Pts',(3.24931437407249,-1.35418260005473,1.93143856892221));
#35496=CARTESIAN_POINT('Ctrl Pts',(3.37653320925761,-2.35730644925339,-0.0939656234575078));
#35497=CARTESIAN_POINT('Ctrl Pts',(3.50375204444272,-1.19567276206334,-2.03345149280708));
#35498=CARTESIAN_POINT('Ctrl Pts',(3.63097087962784,1.06218487084523,-2.10555757687806));
#35499=CARTESIAN_POINT('Ctrl Pts',(3.75818971481294,2.34767634475008,-0.24602754821659));
#35500=CARTESIAN_POINT('Ctrl Pts',(3.88540854999806,1.47255700028443,1.84196585343814));
#35501=CARTESIAN_POINT('Ctrl Pts',(3.97022110678813,-0.00392161485078923,
2.10247393208426));
#35502=CARTESIAN_POINT('Ctrl Pts',(4.01262738518317,-0.633855508764068,
1.89136320058032));
#35503=CARTESIAN_POINT('Ctrl Pts',(3.7495,-0.778675485261984,2.32349192782157));
#35504=CARTESIAN_POINT('Ctrl Pts',(3.70709372160496,-0.00481760480854909,
2.58283613012782));
#35505=CARTESIAN_POINT('Ctrl Pts',(3.66468744320993,0.902090741196932,2.42282233222775));
#35506=CARTESIAN_POINT('Ctrl Pts',(3.62228116481489,1.53472191663215,1.91530757258047));
#35507=CARTESIAN_POINT('Ctrl Pts',(3.57987488641985,2.16735309206736,1.4077928129332));
#35508=CARTESIAN_POINT('Ctrl Pts',(3.53746860802481,2.5257070969323,0.552777091538723));
#35509=CARTESIAN_POINT('Ctrl Pts',(3.49506232962977,2.44168513067164,-0.255461715829768));
#35510=CARTESIAN_POINT('Ctrl Pts',(3.45265605123473,2.35766316441098,-1.06370052319826));
#35511=CARTESIAN_POINT('Ctrl Pts',(3.4102497728397,1.8312652270247,-1.82516241654077));
#35512=CARTESIAN_POINT('Ctrl Pts',(3.36784349444466,1.10577941123774,-2.19112994599049));
#35513=CARTESIAN_POINT('Ctrl Pts',(3.32543721604962,0.380293595450769,-2.55709747544022));
#35514=CARTESIAN_POINT('Ctrl Pts',(3.28303093765459,-0.544280098736887,
-2.52757064099715));
#35515=CARTESIAN_POINT('Ctrl Pts',(3.24062465925955,-1.24440655400711,-2.11570565525482));
#35516=CARTESIAN_POINT('Ctrl Pts',(3.19821838086451,-1.94453300927732,-1.70384066951249));
#35517=CARTESIAN_POINT('Ctrl Pts',(3.15581210246947,-2.42021222563011,-0.909637532470912));
#35518=CARTESIAN_POINT('Ctrl Pts',(3.11340582407443,-2.45266644779647,-0.0978429804161414));
#35519=CARTESIAN_POINT('Ctrl Pts',(3.11171304812031,-2.45396195706944,-0.0654377246516965));
#35520=CARTESIAN_POINT('Ctrl Pts',(3.11002027216618,-2.45455120914745,-0.0330044378339819));
#35521=CARTESIAN_POINT('Ctrl Pts',(3.10832749621205,-2.45444621147543,-0.000567327939743623));
#35522=CARTESIAN_POINT('Origin',(4.,0.,1.44337567297406));
#35523=CARTESIAN_POINT('',(4.,8.83812698937422E-17,1.44337567297406));
#35524=CARTESIAN_POINT('',(4.,1.25,0.721687836487032));
#35525=CARTESIAN_POINT('',(4.,0.3125,1.26295371385231));
#35526=CARTESIAN_POINT('',(1.8,1.38777878078145E-16,1.44337567297406));
#35527=CARTESIAN_POINT('',(4.,8.83812698937422E-17,1.44337567297406));
#35528=CARTESIAN_POINT('',(1.8,1.25,0.721687836487032));
#35529=CARTESIAN_POINT('',(1.8,1.25,0.721687836487032));
#35530=CARTESIAN_POINT('',(4.,1.25,0.721687836487032));
#35531=CARTESIAN_POINT('Origin',(4.,-1.25,0.721687836487032));
#35532=CARTESIAN_POINT('',(4.,-1.25,0.721687836487032));
#35533=CARTESIAN_POINT('',(4.,-0.9375,0.90210979560879));
#35534=CARTESIAN_POINT('',(1.8,-1.25,0.721687836487032));
#35535=CARTESIAN_POINT('',(4.,-1.25,0.721687836487032));
#35536=CARTESIAN_POINT('',(1.8,8.83812698937422E-17,1.44337567297406));
#35537=CARTESIAN_POINT('Origin',(4.,-1.25,-0.721687836487032));
#35538=CARTESIAN_POINT('',(4.,-1.25,-0.721687836487032));
#35539=CARTESIAN_POINT('',(4.,-1.25,-0.360843918243516));
#35540=CARTESIAN_POINT('',(1.8,-1.25,-0.721687836487032));
#35541=CARTESIAN_POINT('',(4.,-1.25,-0.721687836487032));
#35542=CARTESIAN_POINT('',(1.8,-1.25,0.721687836487032));
#35543=CARTESIAN_POINT('Origin',(4.,-2.77555756156289E-16,-1.44337567297406));
#35544=CARTESIAN_POINT('',(4.,-2.65143809681227E-16,-1.44337567297406));
#35545=CARTESIAN_POINT('',(4.,-0.3125,-1.26295371385231));
#35546=CARTESIAN_POINT('',(1.8,-2.77555756156289E-16,-1.44337567297406));
#35547=CARTESIAN_POINT('',(4.,-2.65143809681227E-16,-1.44337567297406));
#35548=CARTESIAN_POINT('',(1.8,-1.25,-0.721687836487032));
#35549=CARTESIAN_POINT('Origin',(4.,1.25,-0.721687836487033));
#35550=CARTESIAN_POINT('',(4.,1.25,-0.721687836487033));
#35551=CARTESIAN_POINT('',(4.,0.9375,-0.902109795608791));
#35552=CARTESIAN_POINT('',(1.8,1.25,-0.721687836487033));
#35553=CARTESIAN_POINT('',(4.,1.25,-0.721687836487033));
#35554=CARTESIAN_POINT('',(1.8,-2.65143809681227E-16,-1.44337567297406));
#35555=CARTESIAN_POINT('Origin',(4.,1.25,0.721687836487032));
#35556=CARTESIAN_POINT('',(4.,1.25,0.360843918243516));
#35557=CARTESIAN_POINT('',(1.8,1.25,-0.721687836487033));
#35558=CARTESIAN_POINT('Origin',(1.8,0.,0.));
#35559=CARTESIAN_POINT('Origin',(0.,2.,0.));
#35560=CARTESIAN_POINT('',(6.93889390390723E-17,-2.,-2.44929359829471E-16));
#35561=CARTESIAN_POINT('Origin',(0.,0.,0.));
#35562=CARTESIAN_POINT('Origin',(0.25,0.,0.));
#35563=CARTESIAN_POINT('',(0.25,-2.25,-2.75545529808154E-16));
#35564=CARTESIAN_POINT('Origin',(2.1,0.,0.));
#35565=CARTESIAN_POINT('Origin',(3.7495,0.,0.));
#35566=CARTESIAN_POINT('Origin',(3.85,0.,0.));
#35567=CARTESIAN_POINT('',(4.,-2.2,-2.69422295812418E-16));
#35568=CARTESIAN_POINT('Origin',(4.,0.,0.));
#35569=CARTESIAN_POINT('',(3.85,-2.35,-2.87791997799628E-16));
#35570=CARTESIAN_POINT('Origin',(4.,0.,0.));
#35571=CARTESIAN_POINT('',(0.,0.,0.));
#35572=CARTESIAN_POINT('Origin',(-5.8,0.,0.));
#35573=CARTESIAN_POINT('',(-11.3916725037879,-2.45326874606972,0.00165903621109187));
#35574=CARTESIAN_POINT('',(-11.5073274962121,-2.45271280748372,0.00261884364159621));
#35575=CARTESIAN_POINT('',(-5.8,-2.4505,-3.00099698131059E-16));
#35576=CARTESIAN_POINT('',(-11.6495,1.0763698230184,2.20363939945498));
#35577=CARTESIAN_POINT('Ctrl Pts',(-11.3916725037879,-2.45326874606972,
0.00165903621109187));
#35578=CARTESIAN_POINT('Ctrl Pts',(-11.396350692832,-2.45391416980342,0.0913991870340253));
#35579=CARTESIAN_POINT('Ctrl Pts',(-11.401028881876,-2.44941587367896,0.181069995962132));
#35580=CARTESIAN_POINT('Ctrl Pts',(-11.4057070709201,-2.43955857964069,
0.270142727834855));
#35581=CARTESIAN_POINT('Ctrl Pts',(-11.447950430442,-2.35054866318539,1.07445640577286));
#35582=CARTESIAN_POINT('Ctrl Pts',(-11.4901937899639,-1.82457545773628,
1.83000392977773));
#35583=CARTESIAN_POINT('Ctrl Pts',(-11.5324371494858,-1.10120406205714,
2.19334617876553));
#35584=CARTESIAN_POINT('Ctrl Pts',(-11.5714580996572,-0.433012907147874,
2.52897194227881));
#35585=CARTESIAN_POINT('Ctrl Pts',(-11.6104790498286,0.403609217336298,
2.52994664001211));
#35586=CARTESIAN_POINT('Ctrl Pts',(-11.6495,1.07765118568551,2.20520362934388));
#35587=CARTESIAN_POINT('',(-11.6495,-1.07508846035132,2.20207516956607));
#35588=CARTESIAN_POINT('Origin',(-11.6495,0.,0.));
#35589=CARTESIAN_POINT('Ctrl Pts',(-11.6495,-1.07508846035132,2.20207516956607));
#35590=CARTESIAN_POINT('Ctrl Pts',(-11.6072566404781,-1.80568981079581,
1.84538385773644));
#35591=CARTESIAN_POINT('Ctrl Pts',(-11.5650132809561,-2.33864379958948,
1.09973146804981));
#35592=CARTESIAN_POINT('Ctrl Pts',(-11.5227699214342,-2.43617762455603,
0.297632529466726));
#35593=CARTESIAN_POINT('Ctrl Pts',(-11.5176224463602,-2.4480624021536,0.199894462702958));
#35594=CARTESIAN_POINT('Ctrl Pts',(-11.5124749712861,-2.4534820068687,0.10131827054319));
#35595=CARTESIAN_POINT('Ctrl Pts',(-11.5073274962121,-2.45271280748372,
0.00261884364159621));
#35596=CARTESIAN_POINT('Origin',(-5.8,0.,0.));
#35597=CARTESIAN_POINT('',(-10.5916725037879,-2.44690286424559,0.000985173157012215));
#35598=CARTESIAN_POINT('',(-10.7073274962121,-2.44679512213092,0.000865365862940725));
#35599=CARTESIAN_POINT('',(-5.8,-2.4505,-3.00099698131059E-16));
#35600=CARTESIAN_POINT('Ctrl Pts',(-10.5916725037879,-2.44690286424559,
0.000985173157012215));
#35601=CARTESIAN_POINT('Ctrl Pts',(-10.6095572023671,-2.44815484704989,
0.346377013341112));
#35602=CARTESIAN_POINT('Ctrl Pts',(-10.6274419009462,-2.37991493328307,
0.691295890238114));
#35603=CARTESIAN_POINT('Ctrl Pts',(-10.6453265995254,-2.23975584232974,
1.00397534838721));
#35604=CARTESIAN_POINT('Ctrl Pts',(-10.6875699590473,-1.90870240896011,
1.74251900945362));
#35605=CARTESIAN_POINT('Ctrl Pts',(-10.7298133185692,-1.1764143924686,2.30120007687742));
#35606=CARTESIAN_POINT('Ctrl Pts',(-10.7720566780912,-0.376649708717779,
2.42540263668847));
#35607=CARTESIAN_POINT('Ctrl Pts',(-10.8143000376131,0.423114975033042,
2.54960519649952));
#35608=CARTESIAN_POINT('Ctrl Pts',(-10.856543397135,1.29035632604318,2.23932924869781));
#35609=CARTESIAN_POINT('Ctrl Pts',(-10.8987867566569,1.82979774721867,1.63595568520028));
#35610=CARTESIAN_POINT('Ctrl Pts',(-10.9410301161789,2.36923916839415,1.03258212170276));
#35611=CARTESIAN_POINT('Ctrl Pts',(-10.9832734757008,2.58088065973499,0.13611094250942));
#35612=CARTESIAN_POINT('Ctrl Pts',(-11.0255168352227,2.36827281982661,-0.644796181245458));
#35613=CARTESIAN_POINT('Ctrl Pts',(-11.0677601947446,2.15566497991823,-1.42570330500034));
#35614=CARTESIAN_POINT('Ctrl Pts',(-11.1100035542666,1.51880780876064,-2.09104637331676));
#35615=CARTESIAN_POINT('Ctrl Pts',(-11.1522469137885,0.747943825078181,
-2.33770810284367));
#35616=CARTESIAN_POINT('Ctrl Pts',(-11.1944902733104,-0.0229201586042772,
-2.58436983237059));
#35617=CARTESIAN_POINT('Ctrl Pts',(-11.2367336328323,-0.927790954811604,
-2.412350223108));
#35618=CARTESIAN_POINT('Ctrl Pts',(-11.2789769923543,-1.55420303918453,
-1.89980050254114));
#35619=CARTESIAN_POINT('Ctrl Pts',(-11.3165421628322,-2.11124388548996,
-1.44401247220008));
#35620=CARTESIAN_POINT('Ctrl Pts',(-11.35410733331,-2.44808608834503,-0.718941185934915));
#35621=CARTESIAN_POINT('Ctrl Pts',(-11.3916725037879,-2.45326874606972,
0.00165903621109187));
#35622=CARTESIAN_POINT('Ctrl Pts',(-11.5073274962121,-2.45271280748372,
0.00261884364159621));
#35623=CARTESIAN_POINT('Ctrl Pts',(-11.4702316117642,-2.44716948166043,
-0.708670183063881));
#35624=CARTESIAN_POINT('Ctrl Pts',(-11.4331357273163,-2.12020852811566,
-1.42635944763925));
#35625=CARTESIAN_POINT('Ctrl Pts',(-11.3960398428684,-1.57526873372546,
-1.88288102370373));
#35626=CARTESIAN_POINT('Ctrl Pts',(-11.3537964833465,-0.954712356788896,
-2.40275015081152));
#35627=CARTESIAN_POINT('Ctrl Pts',(-11.3115531238246,-0.0514859417763487,
-2.58394291754756));
#35628=CARTESIAN_POINT('Ctrl Pts',(-11.2693097643027,0.722133127858049,
-2.34562133189025));
#35629=CARTESIAN_POINT('Ctrl Pts',(-11.2270664047807,1.49575219749244,-2.10729974623295));
#35630=CARTESIAN_POINT('Ctrl Pts',(-11.1848230452588,2.13976392174869,-1.44946380818232));
#35631=CARTESIAN_POINT('Ctrl Pts',(-11.1425796857369,2.36095443699346,-0.671056592573343));
#35632=CARTESIAN_POINT('Ctrl Pts',(-11.100336326215,2.58214495223823,0.107350623035637));
#35633=CARTESIAN_POINT('Ctrl Pts',(-11.058092966693,2.38051425847153,1.00632911620296));
#35634=CARTESIAN_POINT('Ctrl Pts',(-11.0158496071711,1.847797719222,1.61568322182738));
#35635=CARTESIAN_POINT('Ctrl Pts',(-10.9736062476492,1.31508117997247,2.22503732745181));
#35636=CARTESIAN_POINT('Ctrl Pts',(-10.9313628881273,0.451278795240105,
2.54476704553332));
#35637=CARTESIAN_POINT('Ctrl Pts',(-10.8891195286053,-0.349820928189299,
2.42938746378778));
#35638=CARTESIAN_POINT('Ctrl Pts',(-10.8468761690834,-1.15092065161871,
2.31400788204225));
#35639=CARTESIAN_POINT('Ctrl Pts',(-10.8046328095615,-1.88931771374515,
1.76351900046965));
#35640=CARTESIAN_POINT('Ctrl Pts',(-10.7623894500395,-2.22851142489181,
1.02869552114519));
#35641=CARTESIAN_POINT('Ctrl Pts',(-10.7440354654304,-2.37588502927285,
0.709427854401686));
#35642=CARTESIAN_POINT('Ctrl Pts',(-10.7256814808212,-2.44789913409454,
0.355362476156112));
#35643=CARTESIAN_POINT('Ctrl Pts',(-10.7073274962121,-2.44679512213092,
0.000865365862940725));
#35644=CARTESIAN_POINT('Origin',(-5.8,0.,0.));
#35645=CARTESIAN_POINT('',(-9.79167250378794,-2.44974976939592,-0.00219261657894043));
#35646=CARTESIAN_POINT('',(-9.90732749621206,-2.45001435398628,-0.00220888930837992));
#35647=CARTESIAN_POINT('',(-5.8,-2.4505,-3.00099698131059E-16));
#35648=CARTESIAN_POINT('Ctrl Pts',(-9.79167250378794,-2.44974976939592,
-0.00219261657894043));
#35649=CARTESIAN_POINT('Ctrl Pts',(-9.8227637119022,-2.44448661548819,0.596485312663463));
#35650=CARTESIAN_POINT('Ctrl Pts',(-9.85385492001645,-2.22318596315255,
1.19864597202315));
#35651=CARTESIAN_POINT('Ctrl Pts',(-9.88494612813071,-1.82480365830791,
1.64151179239929));
#35652=CARTESIAN_POINT('Ctrl Pts',(-9.92718948765264,-1.28352501551987,
2.24322980867486));
#35653=CARTESIAN_POINT('Ctrl Pts',(-9.96943284717457,-0.415346110241138,
2.55088277676885));
#35654=CARTESIAN_POINT('Ctrl Pts',(-10.0116762066965,0.384035657178238,
2.42424941641526));
#35655=CARTESIAN_POINT('Ctrl Pts',(-10.0539195662184,1.18341742459761,2.29761605606167));
#35656=CARTESIAN_POINT('Ctrl Pts',(-10.0961629257403,1.91400205415762,1.73669636726052));
#35657=CARTESIAN_POINT('Ctrl Pts',(-10.1384062852623,2.24280448406768,0.997144853200805));
#35658=CARTESIAN_POINT('Ctrl Pts',(-10.1806496447842,2.57160691397774,0.257593339141094));
#35659=CARTESIAN_POINT('Ctrl Pts',(-10.2228930043061,2.49862714423785,-0.660590000177178));
#35660=CARTESIAN_POINT('Ctrl Pts',(-10.2651363638281,2.05712805657016,-1.33891529767941));
#35661=CARTESIAN_POINT('Ctrl Pts',(-10.30737972335,1.61562896890247,-2.01724059518164));
#35662=CARTESIAN_POINT('Ctrl Pts',(-10.3496230828719,0.80561056330699,-2.45570785086783));
#35663=CARTESIAN_POINT('Ctrl Pts',(-10.3918664423938,-0.00373849514181471,
-2.45447576463479));
#35664=CARTESIAN_POINT('Ctrl Pts',(-10.4341098019158,-0.813087553590622,
-2.45324367840176));
#35665=CARTESIAN_POINT('Ctrl Pts',(-10.4763531614377,-1.62176726489275,
-2.01231225024949));
#35666=CARTESIAN_POINT('Ctrl Pts',(-10.5185965209596,-2.06119769541993,
-1.33264340881885));
#35667=CARTESIAN_POINT('Ctrl Pts',(-10.5429551819024,-2.31458513870779,
-0.940728015508654));
#35668=CARTESIAN_POINT('Ctrl Pts',(-10.5673138428452,-2.44519768456358,
-0.469432748074029));
#35669=CARTESIAN_POINT('Ctrl Pts',(-10.5916725037879,-2.44690286424559,
0.000985173157012215));
#35670=CARTESIAN_POINT('Ctrl Pts',(-10.7073274962121,-2.44679512213092,
0.000865365862940725));
#35671=CARTESIAN_POINT('Ctrl Pts',(-10.6834381212993,-2.44535815047224,
-0.460544761344943));
#35672=CARTESIAN_POINT('Ctrl Pts',(-10.6595487463865,-2.32004898097106,
-0.922686302325035));
#35673=CARTESIAN_POINT('Ctrl Pts',(-10.6356593714738,-2.07581002964994,
-1.30977971176545));
#35674=CARTESIAN_POINT('Ctrl Pts',(-10.5934160119518,-1.64392456309453,
-1.99427338827529));
#35675=CARTESIAN_POINT('Ctrl Pts',(-10.5511726524299,-0.84016326981684,
-2.44410266421862));
#35676=CARTESIAN_POINT('Ctrl Pts',(-10.508929292908,-0.0308758190729953,
-2.45427970781378));
#35677=CARTESIAN_POINT('Ctrl Pts',(-10.4666859333861,0.778411631670846,
-2.46445675140895));
#35678=CARTESIAN_POINT('Ctrl Pts',(-10.4244425738641,1.59322523988084,-2.03498156265595));
#35679=CARTESIAN_POINT('Ctrl Pts',(-10.3821992143422,2.04219679318729,-1.3615815498271));
#35680=CARTESIAN_POINT('Ctrl Pts',(-10.3399558548203,2.49116834649374,-0.68818153699824));
#35681=CARTESIAN_POINT('Ctrl Pts',(-10.2977124952984,2.57429784489666,0.229143299906478));
#35682=CARTESIAN_POINT('Ctrl Pts',(-10.2554691357764,2.2536932268818,0.972286250652608));
#35683=CARTESIAN_POINT('Ctrl Pts',(-10.2132257762545,1.93308860886695,1.71542920139874));
#35684=CARTESIAN_POINT('Ctrl Pts',(-10.1709824167326,1.20874987443433,2.28439026598628));
#35685=CARTESIAN_POINT('Ctrl Pts',(-10.1287390572107,0.410816991349512,
2.41985411814018));
#35686=CARTESIAN_POINT('Ctrl Pts',(-10.0864956976887,-0.387115891735307,
2.55531797029409));
#35687=CARTESIAN_POINT('Ctrl Pts',(-10.0442523381668,-1.25864292347232,
2.25728461001436));
#35688=CARTESIAN_POINT('Ctrl Pts',(-10.0020089786449,-1.80654156532024,
1.66158866780937));
#35689=CARTESIAN_POINT('Ctrl Pts',(-9.97044848450061,-2.21588286945397,
1.21653745719321));
#35690=CARTESIAN_POINT('Ctrl Pts',(-9.93888799035633,-2.44458276857899,
0.605338316737112));
#35691=CARTESIAN_POINT('Ctrl Pts',(-9.90732749621206,-2.45001435398628,
-0.00220888930837992));
#35692=CARTESIAN_POINT('Origin',(-5.8,0.,0.));
#35693=CARTESIAN_POINT('',(-8.99167250378794,-2.45422282275285,0.000713024433140873));
#35694=CARTESIAN_POINT('',(-9.10732749621206,-2.45409992352044,0.000866640446018732));
#35695=CARTESIAN_POINT('',(-5.8,-2.4505,-3.00099698131059E-16));
#35696=CARTESIAN_POINT('Ctrl Pts',(-8.99167250378794,-2.45422282275285,
0.000713024433140873));
#35697=CARTESIAN_POINT('Ctrl Pts',(-8.99372686191538,-2.45437476902073,
0.0400839655821273));
#35698=CARTESIAN_POINT('Ctrl Pts',(-8.99578122004282,-2.45350899743941,
0.0794480827888193));
#35699=CARTESIAN_POINT('Ctrl Pts',(-8.99783557817026,-2.45160453815159,
0.11876188335754));
#35700=CARTESIAN_POINT('Ctrl Pts',(-9.04007893769219,-2.41244351879692,
0.927163782429675));
#35701=CARTESIAN_POINT('Ctrl Pts',(-9.08232229721412,-1.93409539353615,
1.71429035642438));
#35702=CARTESIAN_POINT('Ctrl Pts',(-9.12456565673604,-1.23458105964887,
2.12138605820959));
#35703=CARTESIAN_POINT('Ctrl Pts',(-9.16680901625797,-0.535066725761605,
2.52848175999481));
#35704=CARTESIAN_POINT('Ctrl Pts',(-9.2090523757799,0.385613816752166,2.55554658957053));
#35705=CARTESIAN_POINT('Ctrl Pts',(-9.25129573530183,1.10783396964644,2.19024498177808));
#35706=CARTESIAN_POINT('Ctrl Pts',(-9.29353909482375,1.83005412254071,1.82494337398563));
#35707=CARTESIAN_POINT('Ctrl Pts',(-9.33578245434568,2.3538138858155,1.06727532882499));
#35708=CARTESIAN_POINT('Ctrl Pts',(-9.3780258138676,2.44039470189646,0.262569802819703));
#35709=CARTESIAN_POINT('Ctrl Pts',(-9.42026917338953,2.52697551797742,-0.542135723185592));
#35710=CARTESIAN_POINT('Ctrl Pts',(-9.46251253291146,2.17637738686455,-1.39387873003553));
#35711=CARTESIAN_POINT('Ctrl Pts',(-9.50475589243338,1.54839548150531,-1.90445284987471));
#35712=CARTESIAN_POINT('Ctrl Pts',(-9.54699925195531,0.920413576146068,
-2.41502696971389));
#35713=CARTESIAN_POINT('Ctrl Pts',(-9.58924261147723,0.0150478965404477,
-2.58443220254231));
#35714=CARTESIAN_POINT('Ctrl Pts',(-9.63148597099916,-0.755055156366603,
-2.33545730519316));
#35715=CARTESIAN_POINT('Ctrl Pts',(-9.67372933052108,-1.52515820927365,
-2.08648240784401));
#35716=CARTESIAN_POINT('Ctrl Pts',(-9.71597269004301,-2.15999863548214,
-1.41912738031729));
#35717=CARTESIAN_POINT('Ctrl Pts',(-9.75821604956493,-2.37022965843771,
-0.637558334325361));
#35718=CARTESIAN_POINT('Ctrl Pts',(-9.7693682009726,-2.42573017319607,-0.431225873197954));
#35719=CARTESIAN_POINT('Ctrl Pts',(-9.78052035238027,-2.4516376178528,-0.216933288179889));
#35720=CARTESIAN_POINT('Ctrl Pts',(-9.79167250378794,-2.44974976939592,
-0.00219261657894043));
#35721=CARTESIAN_POINT('Ctrl Pts',(-9.90732749621206,-2.45001435398628,
-0.00220888930837992));
#35722=CARTESIAN_POINT('Ctrl Pts',(-9.8966446308344,-2.45185288336507,-0.207856652080567));
#35723=CARTESIAN_POINT('Ctrl Pts',(-9.88596176545675,-2.42811056017536,
-0.413085996340104));
#35724=CARTESIAN_POINT('Ctrl Pts',(-9.87527890007909,-2.37713422124245,
-0.611311718253279));
#35725=CARTESIAN_POINT('Ctrl Pts',(-9.83303554055717,-2.17555798335793,
-1.39515763798067));
#35726=CARTESIAN_POINT('Ctrl Pts',(-9.79079218103525,-1.54813525563007,
-2.06949095330521));
#35727=CARTESIAN_POINT('Ctrl Pts',(-9.74854882151333,-0.780832223944534,
-2.32696561304611));
#35728=CARTESIAN_POINT('Ctrl Pts',(-9.7063054619914,-0.013529192258997,
-2.58444027278702));
#35729=CARTESIAN_POINT('Ctrl Pts',(-9.66406210246947,0.893654143384223,
-2.42505627694429));
#35730=CARTESIAN_POINT('Ctrl Pts',(-9.62181874294754,1.52724305817981,-1.92145707918132));
#35731=CARTESIAN_POINT('Ctrl Pts',(-9.57957538342561,2.1608319729754,-1.41785788141836));
#35732=CARTESIAN_POINT('Ctrl Pts',(-9.53733202390369,2.52082646692336,-0.570043481735153));
#35733=CARTESIAN_POINT('Ctrl Pts',(-9.49508866438176,2.44314863923228,0.235570158161625));
#35734=CARTESIAN_POINT('Ctrl Pts',(-9.45284530485984,2.36547081154121,1.04118379805841));
#35735=CARTESIAN_POINT('Ctrl Pts',(-9.41060194533792,1.85012066221109,1.80459667816875));
#35736=CARTESIAN_POINT('Ctrl Pts',(-9.36835858581599,1.13198386014999,2.17786155730722));
#35737=CARTESIAN_POINT('Ctrl Pts',(-9.32611522629406,0.413847058088879,
2.55112643644568));
#35738=CARTESIAN_POINT('Ctrl Pts',(-9.28387186677213,-0.507076396703215,
2.53424331461225));
#35739=CARTESIAN_POINT('Ctrl Pts',(-9.2416285072502,-1.21104920978698,2.13490710462407));
#35740=CARTESIAN_POINT('Ctrl Pts',(-9.19938514772828,-1.91502202287073,
1.73557089463589));
#35741=CARTESIAN_POINT('Ctrl Pts',(-9.15714178820636,-2.40204419424616,
0.953781596492964));
#35742=CARTESIAN_POINT('Ctrl Pts',(-9.11489842868443,-2.45014137152306,
0.145862165020361));
#35743=CARTESIAN_POINT('Ctrl Pts',(-9.11237478452698,-2.45301472633666,
0.0975965636097421));
#35744=CARTESIAN_POINT('Ctrl Pts',(-9.10985114036952,-2.45432158385657,
0.0492377053017148));
#35745=CARTESIAN_POINT('Ctrl Pts',(-9.10732749621206,-2.45409992352044,
0.000866640446018732));
#35746=CARTESIAN_POINT('Origin',(-5.8,0.,0.));
#35747=CARTESIAN_POINT('',(-8.19167250378794,-2.44773723643955,0.00164077392830378));
#35748=CARTESIAN_POINT('',(-8.30732749621206,-2.44755708223661,0.00153710713373167));
#35749=CARTESIAN_POINT('',(-5.8,-2.4505,-3.00099698131059E-16));
#35750=CARTESIAN_POINT('Ctrl Pts',(-8.19167250378794,-2.44773723643955,
0.00164077392830378));
#35751=CARTESIAN_POINT('Ctrl Pts',(-8.2069333714505,-2.44955903509693,0.296108357714686));
#35752=CARTESIAN_POINT('Ctrl Pts',(-8.22219423911305,-2.40039019594895,
0.58998802961355));
#35753=CARTESIAN_POINT('Ctrl Pts',(-8.2374551067756,-2.2975061320399,0.863675152607228));
#35754=CARTESIAN_POINT('Ctrl Pts',(-8.27969846629752,-2.01271442839045,
1.62126402558554));
#35755=CARTESIAN_POINT('Ctrl Pts',(-8.32194182581944,-1.31634122677491,
2.22413178247212));
#35756=CARTESIAN_POINT('Ctrl Pts',(-8.36418518534137,-0.525778614071979,
2.39750412827805));
#35757=CARTESIAN_POINT('Ctrl Pts',(-8.4064285448633,0.264783998630956,2.57087647408397));
#35758=CARTESIAN_POINT('Ctrl Pts',(-8.44867190438523,1.14953602242128,2.31475340880925));
#35759=CARTESIAN_POINT('Ctrl Pts',(-8.49091526390716,1.72522631191578,1.7458703756214));
#35760=CARTESIAN_POINT('Ctrl Pts',(-8.53315862342908,2.30091660141027,1.17698734243355));
#35761=CARTESIAN_POINT('Ctrl Pts',(-8.57540198295101,2.56754515660894,0.295344341332577));
#35762=CARTESIAN_POINT('Ctrl Pts',(-8.61764534247293,2.40358835570123,-0.497224508978201));
#35763=CARTESIAN_POINT('Ctrl Pts',(-8.65988870199485,2.23963155479353,-1.28979335928898));
#35764=CARTESIAN_POINT('Ctrl Pts',(-8.70213206151678,1.64508939777945,-1.99328805880957));
#35765=CARTESIAN_POINT('Ctrl Pts',(-8.74437542103871,0.890941548410939,
-2.28707069285046));
#35766=CARTESIAN_POINT('Ctrl Pts',(-8.78661878056064,0.136793699042435,
-2.58085332689134));
#35767=CARTESIAN_POINT('Ctrl Pts',(-8.82886214008257,-0.776959842680494,
-2.46492389545253));
#35768=CARTESIAN_POINT('Ctrl Pts',(-8.87110549960449,-1.43384965681767,
-1.99212056765834));
#35769=CARTESIAN_POINT('Ctrl Pts',(-8.91129450099898,-2.05879393102198,
-1.54231037701346));
#35770=CARTESIAN_POINT('Ctrl Pts',(-8.95148350239346,-2.45125032799142,
-0.769492903931247));
#35771=CARTESIAN_POINT('Ctrl Pts',(-8.99167250378794,-2.45422282275285,
0.000713024433140873));
#35772=CARTESIAN_POINT('Ctrl Pts',(-9.10732749621206,-2.45409992352044,
0.000866640446018732));
#35773=CARTESIAN_POINT('Ctrl Pts',(-9.0676077808476,-2.45061120446613,-0.760447082120007));
#35774=CARTESIAN_POINT('Ctrl Pts',(-9.02788806548312,-2.06848244655717,
-1.5247845755012));
#35775=CARTESIAN_POINT('Ctrl Pts',(-8.98816835011865,-1.45578892873754,
-1.97614450095185));
#35776=CARTESIAN_POINT('Ctrl Pts',(-8.94592499059672,-0.804167125496714,
-2.45618217064918));
#35777=CARTESIAN_POINT('Ctrl Pts',(-8.9036816310748,0.108248664163322,-2.58220794524156));
#35778=CARTESIAN_POINT('Ctrl Pts',(-8.86143827155288,0.865598741831909,
-2.29678195051135));
#35779=CARTESIAN_POINT('Ctrl Pts',(-8.81919491203095,1.62294881950049,-2.01135595578114));
#35780=CARTESIAN_POINT('Ctrl Pts',(-8.77695155250902,2.22523318517763,-1.31447819172835));
#35781=CARTESIAN_POINT('Ctrl Pts',(-8.7347081929871,2.39794343978572,-0.523770718190494));
#35782=CARTESIAN_POINT('Ctrl Pts',(-8.69246483346517,2.5706536943938,0.266936755347366));
#35783=CARTESIAN_POINT('Ctrl Pts',(-8.65022147394324,2.31378983793283,1.1514739383703));
#35784=CARTESIAN_POINT('Ctrl Pts',(-8.60797811442132,1.74442495103308,1.72668760749301));
#35785=CARTESIAN_POINT('Ctrl Pts',(-8.56573475489939,1.17506006413332,2.30190127661573));
#35786=CARTESIAN_POINT('Ctrl Pts',(-8.52349139537747,0.293194146794787,
2.56779143183821));
#35787=CARTESIAN_POINT('Ctrl Pts',(-8.48124803585554,-0.499237081881421,
2.40317099726176));
#35788=CARTESIAN_POINT('Ctrl Pts',(-8.43900467633361,-1.29166831055762,
2.23855056268531));
#35789=CARTESIAN_POINT('Ctrl Pts',(-8.39676131681168,-1.99466485057149,
1.64341953830992));
#35790=CARTESIAN_POINT('Ctrl Pts',(-8.35451795728976,-2.28781583814602,
0.889025981588753));
#35791=CARTESIAN_POINT('Ctrl Pts',(-8.33878780359719,-2.39697642910899,
0.608112561676078));
#35792=CARTESIAN_POINT('Ctrl Pts',(-8.32305764990463,-2.44930811877369,
0.305115909000908));
#35793=CARTESIAN_POINT('Ctrl Pts',(-8.30732749621206,-2.44755708223661,
0.00153710713373167));
#35794=CARTESIAN_POINT('Origin',(-5.8,0.,0.));
#35795=CARTESIAN_POINT('',(-7.39167250378794,-2.44838374609482,-0.00191884294465761));
#35796=CARTESIAN_POINT('',(-7.50732749621206,-2.44860963519768,-0.00198937388838829));
#35797=CARTESIAN_POINT('',(-5.8,-2.4505,-3.00099698131059E-16));
#35798=CARTESIAN_POINT('Ctrl Pts',(-7.39167250378794,-2.44838374609482,
-0.00191884294465761));
#35799=CARTESIAN_POINT('Ctrl Pts',(-7.4201398809856,-2.44433948481649,0.547011082099126));
#35800=CARTESIAN_POINT('Ctrl Pts',(-7.44860725818326,-2.26174822597498,
1.09838028801556));
#35801=CARTESIAN_POINT('Ctrl Pts',(-7.47707463538092,-1.92273537771643,
1.52563359404597));
#35802=CARTESIAN_POINT('Ctrl Pts',(-7.51931799490285,-1.41966684660092,
2.15964405761116));
#35803=CARTESIAN_POINT('Ctrl Pts',(-7.56156135442478,-0.572154269872277,
2.52034836925077));
#35804=CARTESIAN_POINT('Ctrl Pts',(-7.60380471394671,0.233524154591539,
2.44334517930432));
#35805=CARTESIAN_POINT('Ctrl Pts',(-7.64604807346863,1.03920257905534,2.36634198935787));
#35806=CARTESIAN_POINT('Ctrl Pts',(-7.68829143299055,1.80304685125432,1.85163129782536));
#35807=CARTESIAN_POINT('Ctrl Pts',(-7.73053479251248,2.17691300610121,1.13380728515424));
#35808=CARTESIAN_POINT('Ctrl Pts',(-7.7727781520344,2.5507791609481,0.415983272483111));
#35809=CARTESIAN_POINT('Ctrl Pts',(-7.81502151155633,2.53466719844291,-0.504954061326639));
#35810=CARTESIAN_POINT('Ctrl Pts',(-7.85726487107826,2.1359206082407,-1.20926107656453));
#35811=CARTESIAN_POINT('Ctrl Pts',(-7.89950823060019,1.73717401803849,-1.91356809180241));
#35812=CARTESIAN_POINT('Ctrl Pts',(-7.94175159012211,0.955792800139277,
-2.40124478846844));
#35813=CARTESIAN_POINT('Ctrl Pts',(-7.98399494964404,0.147913886306987,
-2.45001850569757));
#35814=CARTESIAN_POINT('Ctrl Pts',(-8.02623830916596,-0.659965027525304,
-2.4987922229267));
#35815=CARTESIAN_POINT('Ctrl Pts',(-8.06848166868789,-1.49434163729067,
-2.10866296071894));
#35816=CARTESIAN_POINT('Ctrl Pts',(-8.11072502820981,-1.97492483933168,
-1.45744333508004));
#35817=CARTESIAN_POINT('Ctrl Pts',(-8.13770752006919,-2.28189219428585,
-1.04148379856765));
#35818=CARTESIAN_POINT('Ctrl Pts',(-8.16469001192857,-2.44451614386937,
-0.519002570739646));
#35819=CARTESIAN_POINT('Ctrl Pts',(-8.19167250378794,-2.44773723643955,
0.00164077392830378));
#35820=CARTESIAN_POINT('Ctrl Pts',(-8.30732749621206,-2.44755708223661,
0.00153710713373167));
#35821=CARTESIAN_POINT('Ctrl Pts',(-8.2808142903827,-2.44460570661564,-0.510145576751263));
#35822=CARTESIAN_POINT('Ctrl Pts',(-8.25430108455334,-2.28800979144261,
-1.02348209820766));
#35823=CARTESIAN_POINT('Ctrl Pts',(-8.22778787872398,-1.99091904313351,
-1.43551728262218));
#35824=CARTESIAN_POINT('Ctrl Pts',(-8.18554451920205,-1.5175658254113,-2.09201090104497));
#35825=CARTESIAN_POINT('Ctrl Pts',(-8.14330115968013,-0.687553954831687,
-2.49134204882359));
#35826=CARTESIAN_POINT('Ctrl Pts',(-8.1010578001582,0.12081482024383,-2.45150408617989));
#35827=CARTESIAN_POINT('Ctrl Pts',(-8.05881444063628,0.92918359531935,-2.4116661235362));
#35828=CARTESIAN_POINT('Ctrl Pts',(-8.01657108111435,1.71590927489077,-1.93265905047019));
#35829=CARTESIAN_POINT('Ctrl Pts',(-7.97432772159243,2.12241903526266,-1.23280409796831));
#35830=CARTESIAN_POINT('Ctrl Pts',(-7.9320843620705,2.52892879563455,-0.532949145466433));
#35831=CARTESIAN_POINT('Ctrl Pts',(-7.88984100254857,2.5552226368069,0.38775368647133));
#35832=CARTESIAN_POINT('Ctrl Pts',(-7.84759764302664,2.1893163855078,1.10966763913623));
#35833=CARTESIAN_POINT('Ctrl Pts',(-7.80535428350472,1.82341013420869,1.83158159180114));
#35834=CARTESIAN_POINT('Ctrl Pts',(-7.7631109239828,1.06530379043812,2.3547066651932));
#35835=CARTESIAN_POINT('Ctrl Pts',(-7.72086756446087,0.260526093597759,
2.4406135826465));
#35836=CARTESIAN_POINT('Ctrl Pts',(-7.67862420493894,-0.544251603242596,
2.52652050009981));
#35837=CARTESIAN_POINT('Ctrl Pts',(-7.63638084541701,-1.39570065315274,
2.17520926161437));
#35838=CARTESIAN_POINT('Ctrl Pts',(-7.59413748589509,-1.90574869754042,
1.54680005399698));
#35839=CARTESIAN_POINT('Ctrl Pts',(-7.56520082266741,-2.25513114859099,
1.11634031273146));
#35840=CARTESIAN_POINT('Ctrl Pts',(-7.53626415943974,-2.44432013405833,
0.555859618793608));
#35841=CARTESIAN_POINT('Ctrl Pts',(-7.50732749621206,-2.44860963519768,
-0.00198937388838829));
#35842=CARTESIAN_POINT('Origin',(-5.8,0.,0.));
#35843=CARTESIAN_POINT('',(-6.59167250378794,-2.45445842439397,-0.000201612658930761));
#35844=CARTESIAN_POINT('',(-6.70732749621206,-2.45447886332923,-3.55310500964387E-5));
#35845=CARTESIAN_POINT('',(-5.8,-2.4505,-3.00099698131059E-16));
#35846=CARTESIAN_POINT('Ctrl Pts',(-6.59167250378794,-2.45445842439397,
-0.000201612658930761));
#35847=CARTESIAN_POINT('Ctrl Pts',(-6.63334639052071,-2.45351233450644,
0.798256039998315));
#35848=CARTESIAN_POINT('Ctrl Pts',(-6.67502027725348,-2.02724189688927,
1.59758088060811));
#35849=CARTESIAN_POINT('Ctrl Pts',(-6.71669416398626,-1.36328849779505,
2.04105699768142));
#35850=CARTESIAN_POINT('Ctrl Pts',(-6.75893752350818,-0.690262189411743,
2.49059320660392));
#35851=CARTESIAN_POINT('Ctrl Pts',(-6.80118088303011,0.226987328759221,
2.57448891306526));
#35852=CARTESIAN_POINT('Ctrl Pts',(-6.84342424255203,0.970397244894051,
2.25450623931421));
#35853=CARTESIAN_POINT('Ctrl Pts',(-6.88566760207396,1.71380716102889,1.93452356556316));
#35854=CARTESIAN_POINT('Ctrl Pts',(-6.92791096159588,2.2833774751276,1.2106625115997));
#35855=CARTESIAN_POINT('Ctrl Pts',(-6.97015432111781,2.41951015816283,0.412843542460657));
#35856=CARTESIAN_POINT('Ctrl Pts',(-7.01239768063973,2.55564284119806,-0.384975426678379));
#35857=CARTESIAN_POINT('Ctrl Pts',(-7.05464104016167,2.25833789316983,-1.25675231099299));
#35858=CARTESIAN_POINT('Ctrl Pts',(-7.09688439968359,1.66310058290577,-1.80514975753896));
#35859=CARTESIAN_POINT('Ctrl Pts',(-7.13912775920552,1.06786327264172,-2.35354720408493));
#35860=CARTESIAN_POINT('Ctrl Pts',(-7.18137111872744,0.174693600141851,
-2.57856521286225));
#35861=CARTESIAN_POINT('Ctrl Pts',(-7.22361447824936,-0.609320704021191,
-2.37764536372776));
#35862=CARTESIAN_POINT('Ctrl Pts',(-7.26585783777129,-1.39333500818423,
-2.17672551459328));
#35863=CARTESIAN_POINT('Ctrl Pts',(-7.30810119729323,-2.06819394401045,
-1.549867807547));
#35864=CARTESIAN_POINT('Ctrl Pts',(-7.35034455681515,-2.32631116917237,
-0.782780646278478));
#35865=CARTESIAN_POINT('Ctrl Pts',(-7.36412053913942,-2.41048577961199,
-0.532625845751297));
#35866=CARTESIAN_POINT('Ctrl Pts',(-7.37789652146368,-2.45034085199531,
-0.267557960034949));
#35867=CARTESIAN_POINT('Ctrl Pts',(-7.39167250378794,-2.44838374609482,
-0.00191884294465761));
#35868=CARTESIAN_POINT('Ctrl Pts',(-7.50732749621206,-2.44860963519768,
-0.00198937388838829));
#35869=CARTESIAN_POINT('Ctrl Pts',(-7.49402079991781,-2.45058218775034,
-0.25851954342685));
#35870=CARTESIAN_POINT('Ctrl Pts',(-7.48071410362356,-2.41345451229918,
-0.514493193732628));
#35871=CARTESIAN_POINT('Ctrl Pts',(-7.46740740732931,-2.33482408253866,
-0.757010573783298));
#35872=CARTESIAN_POINT('Ctrl Pts',(-7.42516404780739,-2.08520438428399,
-1.52690481719685));
#35873=CARTESIAN_POINT('Ctrl Pts',(-7.38292068828546,-1.41731794890942,
-2.16118612727461));
#35874=CARTESIAN_POINT('Ctrl Pts',(-7.34067732876353,-0.63557320140634,
-2.37076258003248));
#35875=CARTESIAN_POINT('Ctrl Pts',(-7.2984339692416,0.146171546096736,-2.58033903279034));
#35876=CARTESIAN_POINT('Ctrl Pts',(-7.25619060971968,1.04177460572832,-2.36521062822831));
#35877=CARTESIAN_POINT('Ctrl Pts',(-7.21394725019776,1.64303916084166,-1.82342831533501));
#35878=CARTESIAN_POINT('Ctrl Pts',(-7.17170389067583,2.24430371595499,-1.28164600244171));
#35879=CARTESIAN_POINT('Ctrl Pts',(-7.1294605311539,2.55122976655008,-0.413209781217136));
#35880=CARTESIAN_POINT('Ctrl Pts',(-7.08721717163197,2.42392694998131,0.386065598544276));
#35881=CARTESIAN_POINT('Ctrl Pts',(-7.04497381211005,2.29662413341254,1.18534097830569));
#35882=CARTESIAN_POINT('Ctrl Pts',(-7.00273045258812,1.73509244967992,1.91545551660394));
#35883=CARTESIAN_POINT('Ctrl Pts',(-6.9604870930662,0.995266091147326,2.24363854331265));
#35884=CARTESIAN_POINT('Ctrl Pts',(-6.91824373354427,0.255439732614725,
2.57182157002137));
#35885=CARTESIAN_POINT('Ctrl Pts',(-6.87600037402234,-0.662681300717852,
2.49807308514054));
#35886=CARTESIAN_POINT('Ctrl Pts',(-6.83375701450042,-1.34063697896121,
2.05600607875245));
#35887=CARTESIAN_POINT('Ctrl Pts',(-6.79161384173763,-2.01698477887735,
1.61498750367272));
#35888=CARTESIAN_POINT('Ctrl Pts',(-6.74947066897485,-2.45430505252168,
0.807395385780097));
#35889=CARTESIAN_POINT('Ctrl Pts',(-6.70732749621206,-2.45447861156877,
-3.55288018881491E-5));
#35890=CARTESIAN_POINT('Origin',(-5.8,0.,0.));
#35891=CARTESIAN_POINT('',(-5.79167250378794,-2.44894776685357,0.00207433421441847));
#35892=CARTESIAN_POINT('',(-5.90732749621206,-2.44870895001949,0.00201676521443267));
#35893=CARTESIAN_POINT('',(-5.8,-2.4505,-3.00099698131059E-16));
#35894=CARTESIAN_POINT('Ctrl Pts',(-5.79167250378794,-2.44894776685357,
0.00207433421441847));
#35895=CARTESIAN_POINT('Ctrl Pts',(-5.80430954053389,-2.45092058764,0.245609603055973));
#35896=CARTESIAN_POINT('Ctrl Pts',(-5.81694657727985,-2.4175077934881,0.48861571488764));
#35897=CARTESIAN_POINT('Ctrl Pts',(-5.8295836140258,-2.34647756527096,0.720077934452022));
#35898=CARTESIAN_POINT('Ctrl Pts',(-5.87182697354773,-2.10903618341683,
1.49381484393203));
#35899=CARTESIAN_POINT('Ctrl Pts',(-5.91407033306966,-1.45124042784645,
2.13855503354418));
#35900=CARTESIAN_POINT('Ctrl Pts',(-5.95631369259159,-0.672899606421731,
2.36043964457516));
#35901=CARTESIAN_POINT('Ctrl Pts',(-5.99855705211351,0.105441215002987,
2.58232425560614));
#35902=CARTESIAN_POINT('Ctrl Pts',(-6.04080041163544,1.00432710228205,2.38135328805594));
#35903=CARTESIAN_POINT('Ctrl Pts',(-6.08304377115736,1.61406499578435,1.84912503238377));
#35904=CARTESIAN_POINT('Ctrl Pts',(-6.12528713067929,2.22380288928667,1.31689677671159));
#35905=CARTESIAN_POINT('Ctrl Pts',(-6.16753049020121,2.54439278901222,0.453411232917425));
#35906=CARTESIAN_POINT('Ctrl Pts',(-6.20977384972314,2.4297166406405,-0.347773262628461));
#35907=CARTESIAN_POINT('Ctrl Pts',(-6.25201720924507,2.31504049226878,-1.14895775817434));
#35908=CARTESIAN_POINT('Ctrl Pts',(-6.29426056876699,1.7650982957998,-1.88784120547194));
#35909=CARTESIAN_POINT('Ctrl Pts',(-6.33650392828892,1.03054200192067,-2.22765625227097));
#35910=CARTESIAN_POINT('Ctrl Pts',(-6.37874728781084,0.295985708041539,
-2.56747129907001));
#35911=CARTESIAN_POINT('Ctrl Pts',(-6.42099064733277,-0.623184683247735,
-2.50821794537048));
#35912=CARTESIAN_POINT('Ctrl Pts',(-6.4632340068547,-1.30803086703115,-2.07690260891029));
#35913=CARTESIAN_POINT('Ctrl Pts',(-6.50547736637662,-1.99287705081456,
-1.6455872724501));
#35914=CARTESIAN_POINT('Ctrl Pts',(-6.54772072589855,-2.44339902709211,
-0.842209953229236));
#35915=CARTESIAN_POINT('Ctrl Pts',(-6.58996408542048,-2.45425846593306,
-0.03293293792698));
#35916=CARTESIAN_POINT('Ctrl Pts',(-6.59053355820963,-2.45440485947267,
-0.0220232649199538));
#35917=CARTESIAN_POINT('Ctrl Pts',(-6.59110303099879,-2.45447135269246,
-0.0111125197551619));
#35918=CARTESIAN_POINT('Ctrl Pts',(-6.59167250378794,-2.45445842439397,
-0.000201612658930761));
#35919=CARTESIAN_POINT('Ctrl Pts',(-6.70732749621206,-2.45447861156877,
-3.55288018881219E-5));
#35920=CARTESIAN_POINT('Ctrl Pts',(-6.70722730945292,-2.45447902416985,
-0.00195503037850885));
#35921=CARTESIAN_POINT('Ctrl Pts',(-6.70712712269378,-2.45447696622223,
-0.00387453104408387));
#35922=CARTESIAN_POINT('Ctrl Pts',(-6.70702693593464,-2.45447243506411,
-0.00579402587139999));
#35923=CARTESIAN_POINT('Ctrl Pts',(-6.66478357641271,-2.45256188976951,
-0.815141596211808));
#35924=CARTESIAN_POINT('Ctrl Pts',(-6.62254021689079,-2.01095047602618,
-1.62345120899729));
#35925=CARTESIAN_POINT('Ctrl Pts',(-6.58029685736886,-1.33091527897354,
-2.06231254309822));
#35926=CARTESIAN_POINT('Ctrl Pts',(-6.53805349784693,-0.650880081920891,
-2.50117387719915));
#35927=CARTESIAN_POINT('Ctrl Pts',(-6.49581013832501,0.267578898441061,
-2.57058693261554));
#35928=CARTESIAN_POINT('Ctrl Pts',(-6.45356677880308,1.00584760315856,-2.23891471575975));
#35929=CARTESIAN_POINT('Ctrl Pts',(-6.41132341928116,1.74411630787607,-1.90724249890396));
#35930=CARTESIAN_POINT('Ctrl Pts',(-6.36908005975923,2.30219473694912,-1.17448500977598));
#35931=CARTESIAN_POINT('Ctrl Pts',(-6.32683670023731,2.42572261800414,-0.374617519249364));
#35932=CARTESIAN_POINT('Ctrl Pts',(-6.28459334071538,2.54925049905916,0.425249971277239));
#35933=CARTESIAN_POINT('Ctrl Pts',(-6.24234998119346,2.23822783209618,1.29222746320248));
#35934=CARTESIAN_POINT('Ctrl Pts',(-6.20010662167153,1.6344121303279,1.83116506450468));
#35935=CARTESIAN_POINT('Ctrl Pts',(-6.1578632621496,1.03059642855962,2.37010266580688));
#35936=CARTESIAN_POINT('Ctrl Pts',(-6.11561990262767,0.133987691986036,
2.58100037648602));
#35937=CARTESIAN_POINT('Ctrl Pts',(-6.07337654310574,-0.646758896596811,
2.36773550780029));
#35938=CARTESIAN_POINT('Ctrl Pts',(-6.03113318358382,-1.42750548517965,
2.15447063911456));
#35939=CARTESIAN_POINT('Ctrl Pts',(-5.98888982406189,-2.09238992577176,
1.51704319106397));
#35940=CARTESIAN_POINT('Ctrl Pts',(-5.94664646453997,-2.33837203872158,
0.74597903036914));
#35941=CARTESIAN_POINT('Ctrl Pts',(-5.933540141764,-2.41468985543694,0.506750524743217));
#35942=CARTESIAN_POINT('Ctrl Pts',(-5.92043381898803,-2.45068423041799,
0.254658179887264));
#35943=CARTESIAN_POINT('Ctrl Pts',(-5.90732749621206,-2.44870895001949,
0.00201676521443284));
#35944=CARTESIAN_POINT('Origin',(-5.8,0.,0.));
#35945=CARTESIAN_POINT('',(-4.99167250378794,-2.44732265144935,-0.00137759639247254));
#35946=CARTESIAN_POINT('',(-5.10732749621206,-2.44748408483923,-0.00149075522941132));
#35947=CARTESIAN_POINT('',(-5.8,-2.4505,-3.00099698131059E-16));
#35948=CARTESIAN_POINT('Ctrl Pts',(-4.99167250378794,-2.44732265144935,
-0.00137759639247254));
#35949=CARTESIAN_POINT('Ctrl Pts',(-5.01751605006901,-2.44475955460895,
0.497501199516291));
#35950=CARTESIAN_POINT('Ctrl Pts',(-5.04335959635007,-2.29653477948369,
0.9977790446417));
#35951=CARTESIAN_POINT('Ctrl Pts',(-5.06920314263114,-2.01332067653255,
1.40392629772763));
#35952=CARTESIAN_POINT('Ctrl Pts',(-5.11144650215306,-1.55038439671517,
2.06780672049767));
#35953=CARTESIAN_POINT('Ctrl Pts',(-5.15368986167499,-0.726776374453026,
2.48018396746088));
#35954=CARTESIAN_POINT('Ctrl Pts',(-5.19593322119691,0.0821203796264817,
2.45310526460945));
#35955=CARTESIAN_POINT('Ctrl Pts',(-5.23817658071884,0.89101713370599,2.42602656175802));
#35956=CARTESIAN_POINT('Ctrl Pts',(-5.28041994024077,1.68520261960285,1.95949190909194));
#35957=CARTESIAN_POINT('Ctrl Pts',(-5.3226632997627,2.10270399266982,1.266137873699));
#35958=CARTESIAN_POINT('Ctrl Pts',(-5.36490665928462,2.52020536573677,0.572783838306069));
#35959=CARTESIAN_POINT('Ctrl Pts',(-5.40715001880655,2.56102262597383,-0.347389579813734));
#35960=CARTESIAN_POINT('Ctrl Pts',(-5.44939337832847,2.20655213473348,-1.07498691745887));
#35961=CARTESIAN_POINT('Ctrl Pts',(-5.49163673785039,1.85208164349313,-1.80258425510401));
#35962=CARTESIAN_POINT('Ctrl Pts',(-5.53388009737232,1.10232340077537,-2.3376055122745));
#35963=CARTESIAN_POINT('Ctrl Pts',(-5.57612345689425,0.299001259173409,
-2.4361993849062));
#35964=CARTESIAN_POINT('Ctrl Pts',(-5.61836681641618,-0.504320882428552,
-2.53479325753789));
#35965=CARTESIAN_POINT('Ctrl Pts',(-5.66061017593811,-1.3612069229147,-2.19695974563081));
#35966=CARTESIAN_POINT('Ctrl Pts',(-5.70285353546003,-1.88110643908884,
-1.57667617500333));
#35967=CARTESIAN_POINT('Ctrl Pts',(-5.732459858236,-2.24547880580207,-1.14194949103548));
#35968=CARTESIAN_POINT('Ctrl Pts',(-5.76206618101197,-2.4443257996823,-0.568485356447488));
#35969=CARTESIAN_POINT('Ctrl Pts',(-5.79167250378794,-2.44894776685357,
0.00207433421441847));
#35970=CARTESIAN_POINT('Ctrl Pts',(-5.90732749621206,-2.44870895001949,
0.00201676521443267));
#35971=CARTESIAN_POINT('Ctrl Pts',(-5.8781904594661,-2.4443176483143,-0.559637507208111));
#35972=CARTESIAN_POINT('Ctrl Pts',(-5.84905342272015,-2.25226894435809,
-1.12400544701741));
#35973=CARTESIAN_POINT('Ctrl Pts',(-5.81991638597419,-1.89842474885524,
-1.55578018311049));
#35974=CARTESIAN_POINT('Ctrl Pts',(-5.77767302645226,-1.38541556073153,
-2.18177436255622));
#35975=CARTESIAN_POINT('Ctrl Pts',(-5.73542966693034,-0.532317399176566,
-2.52906184810862));
#35976=CARTESIAN_POINT('Ctrl Pts',(-5.69318630740841,0.27204574722632,-2.43935639393703));
#35977=CARTESIAN_POINT('Ctrl Pts',(-5.65094294788649,1.07640889362921,-2.34965093976544));
#35978=CARTESIAN_POINT('Ctrl Pts',(-5.60869958836456,1.83203702488002,-1.82295254586987));
#35979=CARTESIAN_POINT('Ctrl Pts',(-5.56645622884264,2.19453091810013,-1.09931913233965));
#35980=CARTESIAN_POINT('Ctrl Pts',(-5.52421286932071,2.55702481132025,-0.375685718809419));
#35981=CARTESIAN_POINT('Ctrl Pts',(-5.48196950979878,2.52638446650966,0.544882714355476));
#35982=CARTESIAN_POINT('Ctrl Pts',(-5.43972615027686,2.11657510082358,1.24281066450166));
#35983=CARTESIAN_POINT('Ctrl Pts',(-5.39748279075493,1.70676573513749,1.94073861464785));
#35984=CARTESIAN_POINT('Ctrl Pts',(-5.355239431233,0.917787348575927,2.41602608177533));
#35985=CARTESIAN_POINT('Ctrl Pts',(-5.31299607171108,0.109239500713276,
2.45204715221982));
#35986=CARTESIAN_POINT('Ctrl Pts',(-5.27075271218915,-0.699308347149369,
2.4880682226643));
#35987=CARTESIAN_POINT('Ctrl Pts',(-5.22850935266723,-1.52742565631309,
2.08482289642579));
#35988=CARTESIAN_POINT('Ctrl Pts',(-5.1862659931453,-1.99767417913586,1.42610181236799));
#35989=CARTESIAN_POINT('Ctrl Pts',(-5.15995316083422,-2.29058579093952,
1.01579312431041));
#35990=CARTESIAN_POINT('Ctrl Pts',(-5.13364032852314,-2.44464860689455,
0.506362907090105));
#35991=CARTESIAN_POINT('Ctrl Pts',(-5.10732749621206,-2.44748408483923,
-0.00149075522941132));
#35992=CARTESIAN_POINT('Origin',(-5.8,0.,0.));
#35993=CARTESIAN_POINT('',(-4.19167250378794,-2.45388990632559,-0.0010763688550719));
#35994=CARTESIAN_POINT('',(-4.30732749621206,-2.45404119041951,-0.000930649193247773));
#35995=CARTESIAN_POINT('',(-5.8,-2.4505,-3.00099698131059E-16));
#35996=CARTESIAN_POINT('Ctrl Pts',(-4.19167250378794,-2.45388990632559,
-0.0010763688550719));
#35997=CARTESIAN_POINT('Ctrl Pts',(-4.23072255960411,-2.4497607135484,0.747572201937431));
#35998=CARTESIAN_POINT('Ctrl Pts',(-4.26977261542029,-2.08207444069939,
1.49973049661193));
#35999=CARTESIAN_POINT('Ctrl Pts',(-4.30882267123646,-1.48678706708609,
1.95292944397715));
#36000=CARTESIAN_POINT('Ctrl Pts',(-4.35106603075839,-0.842820291192447,
2.44318856572151));
#36001=CARTESIAN_POINT('Ctrl Pts',(-4.39330939028032,0.0674935641221409,
2.58359459469071));
#36002=CARTESIAN_POINT('Ctrl Pts',(-4.43555274980224,0.829252814575512,
2.31015345064403));
#36003=CARTESIAN_POINT('Ctrl Pts',(-4.47779610932417,1.59101206502888,2.03671230659736));
#36004=CARTESIAN_POINT('Ctrl Pts',(-4.5200394688461,2.20421671062104,1.3494239895348));
#36005=CARTESIAN_POINT('Ctrl Pts',(-4.56228282836802,2.38938112254485,0.56153988926041));
#36006=CARTESIAN_POINT('Ctrl Pts',(-4.60452618788995,2.57454553446865,-0.226344211013978));
#36007=CARTESIAN_POINT('Ctrl Pts',(-4.64676954741187,2.3316697127241,-1.11482409450023));
#36008=CARTESIAN_POINT('Ctrl Pts',(-4.6890129069338,1.77145128859989,-1.69894953666164));
#36009=CARTESIAN_POINT('Ctrl Pts',(-4.73125626645573,1.21123286447566,-2.28307497882307));
#36010=CARTESIAN_POINT('Ctrl Pts',(-4.77349962597765,0.333671837971791,
-2.56284597965965));
#36011=CARTESIAN_POINT('Ctrl Pts',(-4.81574298549958,-0.461258149040667,
-2.41074887036126));
#36012=CARTESIAN_POINT('Ctrl Pts',(-4.85798634502151,-1.2561881360531,-2.25865176106287));
#36013=CARTESIAN_POINT('Ctrl Pts',(-4.90022970454343,-1.96848708357411,
-1.67468654162951));
#36014=CARTESIAN_POINT('Ctrl Pts',(-4.94247306406536,-2.27350428864831,
-0.925012132624398));
#36015=CARTESIAN_POINT('Ctrl Pts',(-4.95887287730622,-2.3919187626645,-0.63397182621235));
#36016=CARTESIAN_POINT('Ctrl Pts',(-4.97527269054708,-2.44894914299364,
-0.317956404646919));
#36017=CARTESIAN_POINT('Ctrl Pts',(-4.99167250378794,-2.44732265144935,
-0.00137759639247254));
#36018=CARTESIAN_POINT('Ctrl Pts',(-5.10732749621206,-2.44748408483923,
-0.00149075522941132));
#36019=CARTESIAN_POINT('Ctrl Pts',(-5.09139696900121,-2.4492007627711,-0.308959616470236));
#36020=CARTESIAN_POINT('Ctrl Pts',(-5.07546644179037,-2.39548609667096,
-0.615850602320005));
#36021=CARTESIAN_POINT('Ctrl Pts',(-5.05953591457952,-2.28359309607109,
-0.899817246334982));
#36022=CARTESIAN_POINT('Ctrl Pts',(-5.01729255505759,-1.98688375370171,
-1.65281837910306));
#36023=CARTESIAN_POINT('Ctrl Pts',(-4.97504919553567,-1.28108533248114,
-2.24462380276213));
#36024=CARTESIAN_POINT('Ctrl Pts',(-4.93280583601374,-0.487885733804657,
-2.40550119849799));
#36025=CARTESIAN_POINT('Ctrl Pts',(-4.89056247649182,0.305313864871833,
-2.56637859423385));
#36026=CARTESIAN_POINT('Ctrl Pts',(-4.84831911696989,1.18591464100422,-2.2963279620465));
#36027=CARTESIAN_POINT('Ctrl Pts',(-4.80607575744796,1.7525574995251,-1.71843263355995));
#36028=CARTESIAN_POINT('Ctrl Pts',(-4.76383239792604,2.31920035804599,-1.14053730507339));
#36029=CARTESIAN_POINT('Ctrl Pts',(-4.72158903840411,2.57188529895534,-0.254797280287638));
#36030=CARTESIAN_POINT('Ctrl Pts',(-4.67934567888219,2.39544390318143,0.535085985553977));
#36031=CARTESIAN_POINT('Ctrl Pts',(-4.63710231936026,2.21900250740753,1.32496925139559));
#36032=CARTESIAN_POINT('Ctrl Pts',(-4.59485895983833,1.61343477495037,2.01899575829307));
#36033=CARTESIAN_POINT('Ctrl Pts',(-4.55261560031641,0.854745592120015,
2.30084299289993));
#36034=CARTESIAN_POINT('Ctrl Pts',(-4.51037224079448,0.0960564092896574,
2.58269022750678));
#36035=CARTESIAN_POINT('Ctrl Pts',(-4.46812888127256,-0.815754223913907,
2.45235818982303));
#36036=CARTESIAN_POINT('Ctrl Pts',(-4.42588552175063,-1.46510242369844,
1.96924944923155));
#36037=CARTESIAN_POINT('Ctrl Pts',(-4.38636617990444,-2.07257810212248,
1.51729345699076));
#36038=CARTESIAN_POINT('Ctrl Pts',(-4.34684683805825,-2.45034919829134,
0.756590707680147));
#36039=CARTESIAN_POINT('Ctrl Pts',(-4.30732749621206,-2.45404119041951,
-0.000930649193247773));
#36040=CARTESIAN_POINT('Origin',(-5.8,0.,0.));
#36041=CARTESIAN_POINT('',(-3.39167250378793,-2.45039822849204,0.0022139813149212));
#36042=CARTESIAN_POINT('',(-3.50732749621206,-2.45012855430742,0.00221267815828837));
#36043=CARTESIAN_POINT('',(-5.8,-2.4505,-3.00099698131059E-16));
#36044=CARTESIAN_POINT('Ctrl Pts',(-3.39167250378793,-2.45039822849204,
0.0022139813149212));
#36045=CARTESIAN_POINT('Ctrl Pts',(-3.40168570961729,-2.45214961691583,
0.194893485098156));
#36046=CARTESIAN_POINT('Ctrl Pts',(-3.41169891544666,-2.43132697024435,
0.387198851168568));
#36047=CARTESIAN_POINT('Ctrl Pts',(-3.42171212127602,-2.38648354955538,
0.573729434054478));
#36048=CARTESIAN_POINT('Ctrl Pts',(-3.46395548079794,-2.19729970827227,
1.3606580769851));
#36049=CARTESIAN_POINT('Ctrl Pts',(-3.50619884031987,-1.58059471251749,
2.04480726859311));
#36050=CARTESIAN_POINT('Ctrl Pts',(-3.5484421998418,-0.817449576101223,
2.3143563655275));
#36051=CARTESIAN_POINT('Ctrl Pts',(-3.59068555936372,-0.0543044396849619,
2.58390546246189));
#36052=CARTESIAN_POINT('Ctrl Pts',(-3.63292891888565,0.855280837392778,
2.43885446472266));
#36053=CARTESIAN_POINT('Ctrl Pts',(-3.67517227840757,1.49673664124676,1.94531453054292));
#36054=CARTESIAN_POINT('Ctrl Pts',(-3.7174156379295,2.13819244510074,1.45177459636318));
#36055=CARTESIAN_POINT('Ctrl Pts',(-3.75965899745143,2.51151877573097,0.609745725742923));
#36056=CARTESIAN_POINT('Ctrl Pts',(-3.80190235697336,2.4465614358444,-0.196993240029851));
#36057=CARTESIAN_POINT('Ctrl Pts',(-3.84414571649528,2.38160409595783,-1.00373220580262));
#36058=CARTESIAN_POINT('Ctrl Pts',(-3.8863890760172,1.87836308555447,-1.77518126672792));
#36059=CARTESIAN_POINT('Ctrl Pts',(-3.92863243553913,1.16620494847117,-2.15973035682336));
#36060=CARTESIAN_POINT('Ctrl Pts',(-3.97087579506105,0.454046811387868,
-2.5442794469188));
#36061=CARTESIAN_POINT('Ctrl Pts',(-4.01311915458298,-0.467028452375371,
-2.54192856618438));
#36062=CARTESIAN_POINT('Ctrl Pts',(-4.05536251410491,-1.17721433755474,
-2.15374919604323));
#36063=CARTESIAN_POINT('Ctrl Pts',(-4.09760587362684,-1.88740022273411,
-1.76556982590208));
#36064=CARTESIAN_POINT('Ctrl Pts',(-4.13984923314876,-2.38669672932962,
-0.991561966354189));
#36065=CARTESIAN_POINT('Ctrl Pts',(-4.18209259267069,-2.44753513439102,
-0.184501929320475));
#36066=CARTESIAN_POINT('Ctrl Pts',(-4.18528589637644,-2.45213409400345,
-0.123493812632109));
#36067=CARTESIAN_POINT('Ctrl Pts',(-4.18847920008219,-2.45422756952021,
-0.0622968256623468));
#36068=CARTESIAN_POINT('Ctrl Pts',(-4.19167250378794,-2.45388990632559,
-0.0010763688550719));
#36069=CARTESIAN_POINT('Ctrl Pts',(-4.30732749621206,-2.45404119041951,
-0.000930649193247773));
#36070=CARTESIAN_POINT('Ctrl Pts',(-4.30460347853632,-2.45429567471368,
-0.0531456272134299));
#36071=CARTESIAN_POINT('Ctrl Pts',(-4.30187946086059,-2.45277284613908,
-0.105345489901966));
#36072=CARTESIAN_POINT('Ctrl Pts',(-4.29915544318485,-2.4494254231993,-0.157428083295025));
#36073=CARTESIAN_POINT('Ctrl Pts',(-4.25691208366292,-2.39751445655014,
-0.965111431730932));
#36074=CARTESIAN_POINT('Ctrl Pts',(-4.214668724141,-1.90680675688632,-1.74459268510356));
#36075=CARTESIAN_POINT('Ctrl Pts',(-4.17242536461907,-1.20095645172772,
-2.14060087505314));
#36076=CARTESIAN_POINT('Ctrl Pts',(-4.13018200509715,-0.495106146569108,
-2.53660906500273));
#36077=CARTESIAN_POINT('Ctrl Pts',(-4.08793864557522,0.425886764084292,
-2.54914419152929));
#36078=CARTESIAN_POINT('Ctrl Pts',(-4.04569528605329,1.14225330977148,-2.17249301070089));
#36079=CARTESIAN_POINT('Ctrl Pts',(-4.00345192653137,1.85861985545867,-1.7958418298725));
#36080=CARTESIAN_POINT('Ctrl Pts',(-3.96120856700944,2.37036003617965,-1.03000434168917));
#36081=CARTESIAN_POINT('Ctrl Pts',(-3.91896520748752,2.44423356710959,-0.224032976672993));
#36082=CARTESIAN_POINT('Ctrl Pts',(-3.87672184796559,2.51810709803952,0.581938388343184));
#36083=CARTESIAN_POINT('Ctrl Pts',(-3.83447848844366,2.1541139791784,1.42804363019219));
#36084=CARTESIAN_POINT('Ctrl Pts',(-3.79223512892174,1.5181545285287,1.92864598429309));
#36085=CARTESIAN_POINT('Ctrl Pts',(-3.74999176939981,0.882195077879015,
2.42924833839399));
#36086=CARTESIAN_POINT('Ctrl Pts',(-3.70774840987788,-0.0257307045592446,
2.5843478047468));
#36087=CARTESIAN_POINT('Ctrl Pts',(-3.66550505035596,-0.791809567298263,
2.32325334700692));
#36088=CARTESIAN_POINT('Ctrl Pts',(-3.62326169083403,-1.55788843003727,
2.06215888926704));
#36089=CARTESIAN_POINT('Ctrl Pts',(-3.58101833131211,-2.18212037307705,
1.38487050743447));
#36090=CARTESIAN_POINT('Ctrl Pts',(-3.53877497179018,-2.37999376010142,
0.60008183365056));
#36091=CARTESIAN_POINT('Ctrl Pts',(-3.52829247993081,-2.42909511454254,
0.405340199051181));
#36092=CARTESIAN_POINT('Ctrl Pts',(-3.51780998807143,-2.45194297250802,
0.203979115877225));
#36093=CARTESIAN_POINT('Ctrl Pts',(-3.50732749621206,-2.45012855430742,
0.00221267815828837));
#36094=CARTESIAN_POINT('Origin',(-5.8,0.,0.));
#36095=CARTESIAN_POINT('',(-2.59167250378793,-2.44668279904974,-0.000649636572573609));
#36096=CARTESIAN_POINT('',(-2.70732749621205,-2.44676251251288,-0.000789265007911526));
#36097=CARTESIAN_POINT('',(-5.8,-2.4505,-3.00099698131059E-16));
#36098=CARTESIAN_POINT('Ctrl Pts',(-2.59167250378793,-2.44668279904974,
-0.000649636572573609));
#36099=CARTESIAN_POINT('Ctrl Pts',(-2.6148922191524,-2.44561343820275,0.447872676063153));
#36100=CARTESIAN_POINT('Ctrl Pts',(-2.63811193451688,-2.32764197931026,
0.896918504753983));
#36101=CARTESIAN_POINT('Ctrl Pts',(-2.66133164988135,-2.0962134545358,1.2768548615758));
#36102=CARTESIAN_POINT('Ctrl Pts',(-2.70357500940327,-1.67517821692753,
1.96806867986544));
#36103=CARTESIAN_POINT('Ctrl Pts',(-2.7458183689252,-0.87862160346684,2.43054324988572));
#36104=CARTESIAN_POINT('Ctrl Pts',(-2.78806172844712,-0.0695971627017047,
2.45349249759474));
#36105=CARTESIAN_POINT('Ctrl Pts',(-2.83030508796905,0.739427278063431,
2.47644174530375));
#36106=CARTESIAN_POINT('Ctrl Pts',(-2.87254844749098,1.560919546133,2.05986567070149));
#36107=CARTESIAN_POINT('Ctrl Pts',(-2.9147918070129,2.02046094368866,1.3936307873511));
#36108=CARTESIAN_POINT('Ctrl Pts',(-2.95703516653483,2.48000234124432,0.727395904000699));
#36109=CARTESIAN_POINT('Ctrl Pts',(-2.99927852605676,2.57759286828607,-0.188497788097863));
#36110=CARTESIAN_POINT('Ctrl Pts',(-3.04152188557868,2.26875284079684,-0.936605435506233));
#36111=CARTESIAN_POINT('Ctrl Pts',(-3.08376524510061,1.9599128133076,-1.6847130829146));
#36112=CARTESIAN_POINT('Ctrl Pts',(-3.12600860462254,1.24464223128742,-2.2650346856328));
#36113=CARTESIAN_POINT('Ctrl Pts',(-3.16825196414446,0.448946204655884,
-2.41307200516384));
#36114=CARTESIAN_POINT('Ctrl Pts',(-3.21049532366639,-0.346749821975649,
-2.56110932469487));
#36115=CARTESIAN_POINT('Ctrl Pts',(-3.25273868318831,-1.22287129321851,
-2.27686236103874));
#36116=CARTESIAN_POINT('Ctrl Pts',(-3.29498204271024,-1.78010068543423,
-1.68988483208406));
#36117=CARTESIAN_POINT('Ctrl Pts',(-3.3272121964028,-2.20524653454231,-1.24204223181757));
#36118=CARTESIAN_POINT('Ctrl Pts',(-3.35944235009537,-2.44476092121642,
-0.617976008401615));
#36119=CARTESIAN_POINT('Ctrl Pts',(-3.39167250378793,-2.45039822849204,
0.0022139813149212));
#36120=CARTESIAN_POINT('Ctrl Pts',(-3.50732749621206,-2.45012855430742,
0.00221267815828837));
#36121=CARTESIAN_POINT('Ctrl Pts',(-3.4755666285495,-2.44463105455957,-0.609118788930331));
#36122=CARTESIAN_POINT('Ctrl Pts',(-3.44380576088695,-2.21272709940641,
-1.22417152185401));
#36123=CARTESIAN_POINT('Ctrl Pts',(-3.4120448932244,-1.79867693109158,-1.67009874042576));
#36124=CARTESIAN_POINT('Ctrl Pts',(-3.36980153370247,-1.24797188404843,
-2.26320167498284));
#36125=CARTESIAN_POINT('Ctrl Pts',(-3.32755817418055,-0.375046958953182,
-2.55711857836172));
#36126=CARTESIAN_POINT('Ctrl Pts',(-3.28531481465862,0.422237238642569,
-2.41788838031261));
#36127=CARTESIAN_POINT('Ctrl Pts',(-3.24307145513669,1.21952143623832,-2.27865818226351));
#36128=CARTESIAN_POINT('Ctrl Pts',(-3.20082809561477,1.94116490633457,-1.70628088278641));
#36129=CARTESIAN_POINT('Ctrl Pts',(-3.15858473609284,2.25825791152587,-0.961633875260976));
#36130=CARTESIAN_POINT('Ctrl Pts',(-3.11634137657092,2.57535091671716,-0.216986867735556));
#36131=CARTESIAN_POINT('Ctrl Pts',(-3.07409801704899,2.48789345700351,0.699929847838214));
#36132=CARTESIAN_POINT('Ctrl Pts',(-3.03185465752707,2.03574678129801,1.37120514426048));
#36133=CARTESIAN_POINT('Ctrl Pts',(-2.98961129800514,1.58360010559251,2.04248044068275));
#36134=CARTESIAN_POINT('Ctrl Pts',(-2.94736793848321,0.766764213895166,
2.46811431795353));
#36135=CARTESIAN_POINT('Ctrl Pts',(-2.90512457896129,-0.0424644758308468,
2.45411191152685));
#36136=CARTESIAN_POINT('Ctrl Pts',(-2.86288121943936,-0.851693165556859,
2.44010950510017));
#36137=CARTESIAN_POINT('Ctrl Pts',(-2.82063785991743,-1.65331465331153,
1.98647081497602));
#36138=CARTESIAN_POINT('Ctrl Pts',(-2.77839450039551,-2.08196692368307,
1.29995470395946));
#36139=CARTESIAN_POINT('Ctrl Pts',(-2.75470549900102,-2.32234421245695,
0.914973933129283));
#36140=CARTESIAN_POINT('Ctrl Pts',(-2.73101649760654,-2.44543457696559,
0.456760640272405));
#36141=CARTESIAN_POINT('Ctrl Pts',(-2.70732749621205,-2.44676251251288,
-0.000789265007911525));
#36142=CARTESIAN_POINT('Origin',(-5.8,0.,0.));
#36143=CARTESIAN_POINT('',(-1.79167250378793,-2.45275230455429,-0.00175416635020159));
#36144=CARTESIAN_POINT('',(-1.90732749621205,-2.4529852431004,-0.00165255154954544));
#36145=CARTESIAN_POINT('',(-5.8,-2.4505,-3.00099698131059E-16));
#36146=CARTESIAN_POINT('Ctrl Pts',(-1.79167250378793,-2.45275230455429,
-0.00175416635020159));
#36147=CARTESIAN_POINT('Ctrl Pts',(-1.82809872868751,-2.44708780047584,
0.697443506496413));
#36148=CARTESIAN_POINT('Ctrl Pts',(-1.8645249535871,-2.13271448402931,1.40109234088029));
#36149=CARTESIAN_POINT('Ctrl Pts',(-1.90095117848668,-1.60460482446254,
1.85734002710478));
#36150=CARTESIAN_POINT('Ctrl Pts',(-1.9431945380086,-0.992157987668917,
2.38644879677171));
#36151=CARTESIAN_POINT('Ctrl Pts',(-1.98543789753053,-0.0922580856068916,
2.58282885333754));
#36152=CARTESIAN_POINT('Ctrl Pts',(-2.02768125705246,0.684939924235908,
2.35697404655791));
#36153=CARTESIAN_POINT('Ctrl Pts',(-2.06992461657438,1.46213793407869,2.13111923977828));
#36154=CARTESIAN_POINT('Ctrl Pts',(-2.11216797609631,2.11663405170226,1.48302956965323));
#36155=CARTESIAN_POINT('Ctrl Pts',(-2.15441133561823,2.35012273319099,0.70809067381542));
#36156=CARTESIAN_POINT('Ctrl Pts',(-2.19665469514016,2.58361141467973,-0.0668482220224072));
#36157=CARTESIAN_POINT('Ctrl Pts',(-2.23889805466208,2.39609266003361,-0.968636343572973));
#36158=CARTESIAN_POINT('Ctrl Pts',(-2.28114141418401,1.87303360117565,-1.58625793690777));
#36159=CARTESIAN_POINT('Ctrl Pts',(-2.32338477370594,1.34997454231769,-2.20387953024255));
#36160=CARTESIAN_POINT('Ctrl Pts',(-2.36562813322786,0.491375179247872,
-2.53733459536155));
#36161=CARTESIAN_POINT('Ctrl Pts',(-2.40787149274979,-0.311433207592666,
-2.43464136614626));
#36162=CARTESIAN_POINT('Ctrl Pts',(-2.45011485227172,-1.11424159443319,
-2.33194813693097));
#36163=CARTESIAN_POINT('Ctrl Pts',(-2.49235821179364,-1.86125900504446,
-1.79310661338139));
#36164=CARTESIAN_POINT('Ctrl Pts',(-2.53460157131557,-2.21201077947218,
-1.06370931832713));
#36165=CARTESIAN_POINT('Ctrl Pts',(-2.55362521547302,-2.36996642078062,
-0.735236518162622));
#36166=CARTESIAN_POINT('Ctrl Pts',(-2.57264885963048,-2.4475589140197,-0.368118778133049));
#36167=CARTESIAN_POINT('Ctrl Pts',(-2.59167250378793,-2.44668279904974,
-0.000649636572573609));
#36168=CARTESIAN_POINT('Ctrl Pts',(-2.70732749621205,-2.44676251251288,
-0.000789265007911525));
#36169=CARTESIAN_POINT('Ctrl Pts',(-2.68877313808461,-2.44780261510329,
-0.359164219797027));
#36170=CARTESIAN_POINT('Ctrl Pts',(-2.67021877995717,-2.37414425470941,
-0.717132201493089));
#36171=CARTESIAN_POINT('Ctrl Pts',(-2.65166442182973,-2.22363693076463,
-1.03918588605928));
#36172=CARTESIAN_POINT('Ctrl Pts',(-2.60942106230781,-1.88097161448621,
-1.77241683315251));
#36173=CARTESIAN_POINT('Ctrl Pts',(-2.56717770278588,-1.13995792894096,
-2.31948519543));
#36174=CARTESIAN_POINT('Ctrl Pts',(-2.52493434326395,-0.338334145998326,
-2.4310488509504));
#36175=CARTESIAN_POINT('Ctrl Pts',(-2.48269098374203,0.463289636944311,
-2.54261250647081));
#36176=CARTESIAN_POINT('Ctrl Pts',(-2.4404476242201,1.32552351728434,-2.21867145523413));
#36177=CARTESIAN_POINT('Ctrl Pts',(-2.39820426469818,1.85537964471098,-1.60687114221059));
#36178=CARTESIAN_POINT('Ctrl Pts',(-2.35596090517625,2.38523577213763,-0.995070829187048));
#36179=CARTESIAN_POINT('Ctrl Pts',(-2.31371754565432,2.58271414665089,-0.0954112543766505));
#36180=CARTESIAN_POINT('Ctrl Pts',(-2.2714741861324,2.35780831881423,0.682061905814828));
#36181=CARTESIAN_POINT('Ctrl Pts',(-2.22923082661047,2.13290249097757,1.45953506600631));
#36182=CARTESIAN_POINT('Ctrl Pts',(-2.18698746708854,1.48561246079097,2.11482181157887));
#36183=CARTESIAN_POINT('Ctrl Pts',(-2.14474410756662,0.710959266367213,
2.34925636222754));
#36184=CARTESIAN_POINT('Ctrl Pts',(-2.10250074804469,-0.0636939280565581,
2.58369091287621));
#36185=CARTESIAN_POINT('Ctrl Pts',(-2.06025738852277,-0.965710286717498,
2.39727326860099));
#36186=CARTESIAN_POINT('Ctrl Pts',(-2.01801402900084,-1.58396997886496,
1.87496867400264));
#36187=CARTESIAN_POINT('Ctrl Pts',(-1.98111851807124,-2.12396034627677,
1.41878585387021));
#36188=CARTESIAN_POINT('Ctrl Pts',(-1.94422300714165,-2.44749142227523,
0.706376978662933));
#36189=CARTESIAN_POINT('Ctrl Pts',(-1.90732749621205,-2.4529852431004,-0.00165255154954544));
#36190=CARTESIAN_POINT('Origin',(-5.8,0.,0.));
#36191=CARTESIAN_POINT('',(-0.991672503787933,-2.45191048624635,0.00202700265848121));
#36192=CARTESIAN_POINT('',(-1.10732749621205,-2.45164311140852,0.00208312759044971));
#36193=CARTESIAN_POINT('',(-5.8,-2.4505,-3.00099698131059E-16));
#36194=CARTESIAN_POINT('Ctrl Pts',(-0.991672503787933,-2.45191048624635,
0.00202700265848121));
#36195=CARTESIAN_POINT('Ctrl Pts',(-0.999061878700698,-2.45317470252284,
0.143994484330699));
#36196=CARTESIAN_POINT('Ctrl Pts',(-1.00645125361346,-2.44190225774454,
0.28576134120172));
#36197=CARTESIAN_POINT('Ctrl Pts',(-1.01384062852623,-2.41737842412646,
0.425196841749238));
#36198=CARTESIAN_POINT('Ctrl Pts',(-1.05608398804815,-2.27718129884662,
1.22231757919796));
#36199=CARTESIAN_POINT('Ctrl Pts',(-1.09832734757008,-1.7039093940212,1.94324618025634));
#36200=CARTESIAN_POINT('Ctrl Pts',(-1.14057070709201,-0.958872451732294,
2.25942616043133));
#36201=CARTESIAN_POINT('Ctrl Pts',(-1.18281406661393,-0.213835509443387,
2.57560614060633));
#36202=CARTESIAN_POINT('Ctrl Pts',(-1.22505742613586,0.702966470309022,
2.48703749989794));
#36203=CARTESIAN_POINT('Ctrl Pts',(-1.26730078565778,1.37368755904065,2.03407355411655));
#36204=CARTESIAN_POINT('Ctrl Pts',(-1.30954414517971,2.04440864777229,1.58110960833516));
#36205=CARTESIAN_POINT('Ctrl Pts',(-1.35178750470164,2.46904884548314,0.763750357480772));
#36206=CARTESIAN_POINT('Ctrl Pts',(-1.39403086422356,2.45405941828723,-0.0454617002379226));
#36207=CARTESIAN_POINT('Ctrl Pts',(-1.43627422374549,2.43906999109132,-0.854673757956606));
#36208=CARTESIAN_POINT('Ctrl Pts',(-1.47851758326741,1.98445093898863,-1.65573862253959));
#36209=CARTESIAN_POINT('Ctrl Pts',(-1.52076094278934,1.29741150126341,-2.08355193165779));
#36210=CARTESIAN_POINT('Ctrl Pts',(-1.56300430231127,0.610372063538196,
-2.51136524077598));
#36211=CARTESIAN_POINT('Ctrl Pts',(-1.60524766183319,-0.309087759809568,
-2.56592699442941));
#36212=CARTESIAN_POINT('Ctrl Pts',(-1.64749102135512,-1.04189960834166,
-2.22236703125869));
#36213=CARTESIAN_POINT('Ctrl Pts',(-1.68973438087704,-1.77471145687375,
-1.87880706808797));
#36214=CARTESIAN_POINT('Ctrl Pts',(-1.73197774039897,-2.32087533059018,
-1.13712538809311));
#36215=CARTESIAN_POINT('Ctrl Pts',(-1.7742210999209,-2.43146038168579,-0.335365806711661));
#36216=CARTESIAN_POINT('Ctrl Pts',(-1.78003823454324,-2.44668852965324,
-0.224959260631187));
#36217=CARTESIAN_POINT('Ctrl Pts',(-1.78585536916559,-2.45365690509645,
-0.113413472297838));
#36218=CARTESIAN_POINT('Ctrl Pts',(-1.79167250378793,-2.45275230455429,
-0.00175416635020159));
#36219=CARTESIAN_POINT('Ctrl Pts',(-1.90732749621205,-2.4529852431004,-0.00165255154954544));
#36220=CARTESIAN_POINT('Ctrl Pts',(-1.90197964761972,-2.45378154924243,
-0.104278443726542));
#36221=CARTESIAN_POINT('Ctrl Pts',(-1.89663179902739,-2.44789612195828,
-0.206812329022707));
#36222=CARTESIAN_POINT('Ctrl Pts',(-1.89128395043506,-2.43501963539058,
-0.308460610226293));
#36223=CARTESIAN_POINT('Ctrl Pts',(-1.84904059091313,-2.33330657413478,
-1.11139375493544));
#36224=CARTESIAN_POINT('Ctrl Pts',(-1.80679723139121,-1.79537742598919,
-1.85906849943227));
#36225=CARTESIAN_POINT('Ctrl Pts',(-1.76455387186928,-1.06640896295346,
-2.21071042645277));
#36226=CARTESIAN_POINT('Ctrl Pts',(-1.72231051234736,-0.337440499917736,
-2.56235235347326));
#36227=CARTESIAN_POINT('Ctrl Pts',(-1.68006715282543,0.582567278008129,
-2.51796146301742));
#36228=CARTESIAN_POINT('Ctrl Pts',(-1.6378237933035,1.27429461852628,-2.09777051925233));
#36229=CARTESIAN_POINT('Ctrl Pts',(-1.59558043378158,1.96602195904445,-1.67757957548724));
#36230=CARTESIAN_POINT('Ctrl Pts',(-1.55333707425965,2.42946886215489,-0.881588578412895));
#36231=CARTESIAN_POINT('Ctrl Pts',(-1.51109371473772,2.45340568023822,-0.0725926363383835));
#36232=CARTESIAN_POINT('Ctrl Pts',(-1.4688503552158,2.47734249832155,0.736403305736105));
#36233=CARTESIAN_POINT('Ctrl Pts',(-1.42660699569387,2.06176923137779,1.55840419281076));
#36234=CARTESIAN_POINT('Ctrl Pts',(-1.38436363617195,1.39609611498331,2.01875827328353));
#36235=CARTESIAN_POINT('Ctrl Pts',(-1.34212027665002,0.73042299858883,2.47911235375631));
#36236=CARTESIAN_POINT('Ctrl Pts',(-1.2998769171281,-0.185349967256377,
2.57781962762719));
#36237=CARTESIAN_POINT('Ctrl Pts',(-1.25763355760617,-0.933834445849563,
2.26989378192159));
#36238=CARTESIAN_POINT('Ctrl Pts',(-1.21539019808424,-1.68231892444275,
1.96196793621599));
#36239=CARTESIAN_POINT('Ctrl Pts',(-1.17314683856232,-2.26351491578391,
1.24740897093391));
#36240=CARTESIAN_POINT('Ctrl Pts',(-1.13090347904039,-2.41252280639993,
0.451893154076523));
#36241=CARTESIAN_POINT('Ctrl Pts',(-1.12304481809761,-2.44024319851368,
0.303900921686603));
#36242=CARTESIAN_POINT('Ctrl Pts',(-1.11518615715483,-2.45300629731437,
0.153106910689909));
#36243=CARTESIAN_POINT('Ctrl Pts',(-1.10732749621205,-2.45164311140852,
0.00208312759044971));
#36244=CARTESIAN_POINT('Origin',(-5.8,0.,0.));
#36245=CARTESIAN_POINT('',(-0.191672503787931,-2.44602797108083,-0.000435857851394948));
#36246=CARTESIAN_POINT('',(-0.307327496212056,-2.44646461313235,-7.12799915801969E-5));
#36247=CARTESIAN_POINT('',(-5.8,-2.4505,-3.00099698131059E-16));
#36248=CARTESIAN_POINT('Ctrl Pts',(-0.191672503787931,-2.44601738174545,
-0.0004368899209653));
#36249=CARTESIAN_POINT('Ctrl Pts',(-0.212268388235807,-2.44653079006204,
0.397767213870827));
#36250=CARTESIAN_POINT('Ctrl Pts',(-0.232864272683682,-2.35532542844842,
0.796028585207236));
#36251=CARTESIAN_POINT('Ctrl Pts',(-0.253460157131558,-2.17142533223093,
1.14526153389913));
#36252=CARTESIAN_POINT('Ctrl Pts',(-0.295703516653484,-1.79423551548414,
1.86155866820433));
#36253=CARTESIAN_POINT('Ctrl Pts',(-0.337946876175409,-1.02709377158744,
2.37160106779288));
#36254=CARTESIAN_POINT('Ctrl Pts',(-0.380190235697335,-0.220869436790385,
2.44430655566939));
#36255=CARTESIAN_POINT('Ctrl Pts',(-0.422433595219262,0.585354898006676,
2.5170120435459));
#36256=CARTESIAN_POINT('Ctrl Pts',(-0.464676954741189,1.43066182370407,
2.15238061971035));
#36257=CARTESIAN_POINT('Ctrl Pts',(-0.506920314263115,1.93040321642611,
1.51590454149075));
#36258=CARTESIAN_POINT('Ctrl Pts',(-0.549163673785041,2.43014460914813,
0.879428463271162));
#36259=CARTESIAN_POINT('Ctrl Pts',(-0.591407033306968,2.58432046889479,
-0.0288922693324942));
#36260=CARTESIAN_POINT('Ctrl Pts',(-0.633650392828894,2.32233492104033,
-0.794700919203336));
#36261=CARTESIAN_POINT('Ctrl Pts',(-0.67589375235082,2.06034937318587,-1.56050956907417));
#36262=CARTESIAN_POINT('Ctrl Pts',(-0.718137111872745,1.38220241773032,
-2.18380613621221));
#36263=CARTESIAN_POINT('Ctrl Pts',(-0.760380471394671,0.597149656144279,
-2.38069557645246));
#36264=CARTESIAN_POINT('Ctrl Pts',(-0.802623830916597,-0.187903105441769,
-2.57758501669272));
#36265=CARTESIAN_POINT('Ctrl Pts',(-0.844867190438523,-1.07986167315829,
-2.34806733003518));
#36266=CARTESIAN_POINT('Ctrl Pts',(-0.88711054996045,-1.67227978414943,
-1.79665204978687));
#36267=CARTESIAN_POINT('Ctrl Pts',(-0.921964534569611,-2.16106978466905,
-1.3416925032798));
#36268=CARTESIAN_POINT('Ctrl Pts',(-0.956818519178772,-2.44594746837766,
-0.667601007778074));
#36269=CARTESIAN_POINT('Ctrl Pts',(-0.991672503787933,-2.45191048624635,
0.00202700265848121));
#36270=CARTESIAN_POINT('Ctrl Pts',(-1.10732749621205,-2.45164311140852,
0.00208312759044971));
#36271=CARTESIAN_POINT('Ctrl Pts',(-1.07294279763291,-2.4456786428023,-0.658704670479551));
#36272=CARTESIAN_POINT('Ctrl Pts',(-1.03855809905376,-2.16928017252217,
-1.32389123230908));
#36273=CARTESIAN_POINT('Ctrl Pts',(-1.00417340047461,-1.6920551196339,-1.77803867535403));
#36274=CARTESIAN_POINT('Ctrl Pts',(-0.961930040952687,-1.105759752361,-2.33598201949449));
#36275=CARTESIAN_POINT('Ctrl Pts',(-0.91968668143076,-0.216349227924323,
-2.57539603934272));
#36276=CARTESIAN_POINT('Ctrl Pts',(-0.877443321908835,0.5708124140107,-2.38717728466095));
#36277=CARTESIAN_POINT('Ctrl Pts',(-0.835199962386909,1.35797405594572,
-2.19895852997917));
#36278=CARTESIAN_POINT('Ctrl Pts',(-0.792956602864983,2.04288681537911,
-1.5831070007674));
#36279=CARTESIAN_POINT('Ctrl Pts',(-0.750713243343057,2.31336229750905,
-0.820283519894993));
#36280=CARTESIAN_POINT('Ctrl Pts',(-0.708469883821131,2.583837779639,-0.0574600390225732));
#36281=CARTESIAN_POINT('Ctrl Pts',(-0.666226524299204,2.43987598446552,
0.852335393510467));
#36282=CARTESIAN_POINT('Ctrl Pts',(-0.623983164777278,1.94712925542381,
1.49437790025489));
#36283=CARTESIAN_POINT('Ctrl Pts',(-0.581739805255351,1.4543825263821,2.13642040699932));
#36284=CARTESIAN_POINT('Ctrl Pts',(-0.539496445733424,0.61285086347215,
2.5107099879551));
#36285=CARTESIAN_POINT('Ctrl Pts',(-0.497253086211498,-0.193985232491749,
2.44676681777884));
#36286=CARTESIAN_POINT('Ctrl Pts',(-0.455009726689572,-1.00082132845564,
2.38282364760258));
#36287=CARTESIAN_POINT('Ctrl Pts',(-0.412766367167645,-1.77296185747349,
1.88064772629427));
#36288=CARTESIAN_POINT('Ctrl Pts',(-0.37052300764572,-2.15834482944737,
1.16890388041718));
#36289=CARTESIAN_POINT('Ctrl Pts',(-0.349457837167832,-2.3505207855214,
0.813984062967378));
#36290=CARTESIAN_POINT('Ctrl Pts',(-0.328392666689944,-2.4465240289526,
0.406952230065944));
#36291=CARTESIAN_POINT('Ctrl Pts',(-0.307327496212056,-2.44646461313235,
-7.12799915801969E-5));
#36292=CARTESIAN_POINT('Origin',(-13.1285451186048,0.,0.));
#36293=CARTESIAN_POINT('',(-0.72854511860476,-1.99589816055495,0.00165001573264543));
#36294=CARTESIAN_POINT('',(-0.570454881395212,-1.99146512427903,-5.80231641911233E-5));
#36295=CARTESIAN_POINT('',(-13.1285451186048,-1.99475,-1.92374832954336E-13));
#36296=CARTESIAN_POINT('',(-9.0205620750794E-16,-1.69189910824764,1.06268379792867));
#36297=CARTESIAN_POINT('Ctrl Pts',(-0.72854511860476,-1.99589816055495,
0.00165001573264557));
#36298=CARTESIAN_POINT('Ctrl Pts',(-0.6936911339956,-1.99104415937413,-0.543438935019565));
#36299=CARTESIAN_POINT('Ctrl Pts',(-0.616593789864514,-1.47808926389438,
-1.75721787381682));
#36300=CARTESIAN_POINT('Ctrl Pts',(-0.497253086211501,0.573113500662185,
-2.2850308579914));
#36301=CARTESIAN_POINT('Ctrl Pts',(-0.370523007645721,2.22918406511225,
-0.762907829264197));
#36302=CARTESIAN_POINT('Ctrl Pts',(-0.243792929079945,1.85267849943624,
1.45525921586262));
#36303=CARTESIAN_POINT('Ctrl Pts',(-0.120285259864702,-0.159116251582435,
2.32306659118204));
#36304=CARTESIAN_POINT('Ctrl Pts',(-0.039020950171389,-1.36508286981671,
1.57661195366552));
#36305=CARTESIAN_POINT('Ctrl Pts',(-6.86842076269567E-16,-1.69189910824764,
1.06268379792867));
#36306=CARTESIAN_POINT('',(0.,0.458732584425967,1.94128616604711));
#36307=CARTESIAN_POINT('Origin',(0.,0.,0.));
#36308=CARTESIAN_POINT('Ctrl Pts',(-0.570454881395212,-1.99146512427903,
-5.80231641910539E-5));
#36309=CARTESIAN_POINT('Ctrl Pts',(-0.549276692351179,-1.99141649926868,
-0.333159919088959));
#36310=CARTESIAN_POINT('Ctrl Pts',(-0.48585514378522,-1.75457861196001,
-1.3306674833886));
#36311=CARTESIAN_POINT('Ctrl Pts',(-0.380190235697333,-0.180414554165581,
-2.34831227349832));
#36312=CARTESIAN_POINT('Ctrl Pts',(-0.253460157131555,1.87363647225322,
-1.43076438289222));
#36313=CARTESIAN_POINT('Ctrl Pts',(-0.126730078565778,2.21660082027165,
0.796119646106798));
#36314=CARTESIAN_POINT('Ctrl Pts',(-0.0422433595219261,1.10280973225228,
1.78908852524606));
#36315=CARTESIAN_POINT('Ctrl Pts',(0.,0.458732584425967,1.94128616604711));
#36316=CARTESIAN_POINT('Origin',(-13.1285451186048,0.,0.));
#36317=CARTESIAN_POINT('',(-1.52854511860476,-1.99658341542937,-0.00142792219028397));
#36318=CARTESIAN_POINT('',(-1.37045488139521,-1.99568051274521,0.00169570241191928));
#36319=CARTESIAN_POINT('',(-13.1285451186048,-1.99475,-1.92374832954336E-13));
#36320=CARTESIAN_POINT('Ctrl Pts',(-1.52854511860476,-1.99658341542937,
-0.00142792219028407));
#36321=CARTESIAN_POINT('Ctrl Pts',(-1.52272798398241,-1.99731977614411,
-0.0923205565665347));
#36322=CARTESIAN_POINT('Ctrl Pts',(-1.47466748983814,-1.95045522889083,
-0.842501557985075));
#36323=CARTESIAN_POINT('Ctrl Pts',(-1.38436363617195,-1.00005929055416,
-2.13312382380668));
#36324=CARTESIAN_POINT('Ctrl Pts',(-1.25763355760617,1.24531000055737,-1.9998811491278));
#36325=CARTESIAN_POINT('Ctrl Pts',(-1.13090347904039,2.35551365799275,-0.0436385799048972));
#36326=CARTESIAN_POINT('Ctrl Pts',(-1.00417340047461,1.31851994113852,1.95239573836704));
#36327=CARTESIAN_POINT('Ctrl Pts',(-0.877443321908835,-0.920358755998121,
2.16868502143541));
#36328=CARTESIAN_POINT('Ctrl Pts',(-0.785567227952218,-1.93529438584288,
0.892334100294173));
#36329=CARTESIAN_POINT('Ctrl Pts',(-0.735934493517526,-1.99692725478777,
0.117214036979607));
#36330=CARTESIAN_POINT('Ctrl Pts',(-0.72854511860476,-1.99589816055495,
0.00165001573264557));
#36331=CARTESIAN_POINT('Ctrl Pts',(-1.37045488139521,-1.99568051274521,
0.0016957024119192));
#36332=CARTESIAN_POINT('Ctrl Pts',(-1.33607018281607,-1.99082533063853,
-0.536197160350763));
#36333=CARTESIAN_POINT('Ctrl Pts',(-1.259442124715,-1.48941647468376,-1.74289860347138));
#36334=CARTESIAN_POINT('Ctrl Pts',(-1.14057070709201,0.54788370586334,-2.29130478089007));
#36335=CARTESIAN_POINT('Ctrl Pts',(-1.01384062852623,2.22047671979483,-0.787362926702919));
#36336=CARTESIAN_POINT('Ctrl Pts',(-0.887110549960448,1.86891443749856,
1.43440541328318));
#36337=CARTESIAN_POINT('Ctrl Pts',(-0.760380471394668,-0.186150183504844,
2.34844027344827));
#36338=CARTESIAN_POINT('Ctrl Pts',(-0.654828581872924,-1.75664923517798,
1.3270370721541));
#36339=CARTESIAN_POINT('Ctrl Pts',(-0.591520051873105,-1.99151348979935,
0.331266256243046));
#36340=CARTESIAN_POINT('Ctrl Pts',(-0.570454881395212,-1.99146512427903,
-5.80231641910539E-5));
#36341=CARTESIAN_POINT('Origin',(-13.1285451186048,0.,0.));
#36342=CARTESIAN_POINT('',(-2.32854511860476,-1.99164273144438,-0.000528815569653849));
#36343=CARTESIAN_POINT('',(-2.17045488139521,-1.99677303149338,-0.00134520595961224));
#36344=CARTESIAN_POINT('',(-13.1285451186048,-1.99475,-1.92374832954336E-13));
#36345=CARTESIAN_POINT('Ctrl Pts',(-2.32854511860476,-1.99164273144438,
-0.000528815569653777));
#36346=CARTESIAN_POINT('Ctrl Pts',(-2.3095214744473,-1.99235590440349,-0.299655144942299));
#36347=CARTESIAN_POINT('Ctrl Pts',(-2.24825447076793,-1.7889392995189,-1.26209160177339));
#36348=CARTESIAN_POINT('Ctrl Pts',(-2.14474410756662,-0.298926929475087,
-2.33687315863848));
#36349=CARTESIAN_POINT('Ctrl Pts',(-2.01801402900084,1.79781791380199,-1.52255833577031));
#36350=CARTESIAN_POINT('Ctrl Pts',(-1.89128395043506,2.25574858406966,0.679655729273182));
#36351=CARTESIAN_POINT('Ctrl Pts',(-1.76455387186929,0.657434610640146,
2.26232482066099));
#36352=CARTESIAN_POINT('Ctrl Pts',(-1.64364092792585,-1.43929446373414,
1.80476751535916));
#36353=CARTESIAN_POINT('Ctrl Pts',(-1.56497134350434,-1.991972409712,0.567731252635601));
#36354=CARTESIAN_POINT('Ctrl Pts',(-1.52854511860476,-1.99658341542937,
-0.00142792219028407));
#36355=CARTESIAN_POINT('Ctrl Pts',(-2.17045488139521,-1.99677303149338,
-0.0013452059596123));
#36356=CARTESIAN_POINT('Ctrl Pts',(-2.16510703280289,-1.99742123866611,
-0.0848844830132346));
#36357=CARTESIAN_POINT('Ctrl Pts',(-2.11751582468863,-1.95478691364556,
-0.827644996443922));
#36358=CARTESIAN_POINT('Ctrl Pts',(-2.02768125705245,-1.02358496316198,
-2.12193474222715));
#36359=CARTESIAN_POINT('Ctrl Pts',(-1.90095117848668,1.22312246187489,-2.01352985089457));
#36360=CARTESIAN_POINT('Ctrl Pts',(-1.77422109992089,2.35488419618976,-0.0696779332279315));
#36361=CARTESIAN_POINT('Ctrl Pts',(-1.64749102135512,1.34003240157303,1.9376915050404));
#36362=CARTESIAN_POINT('Ctrl Pts',(-1.52076094278934,-0.896333389432558,
2.17873986401275));
#36363=CARTESIAN_POINT('Ctrl Pts',(-1.42841556280271,-1.93055379041261,
0.907204150401554));
#36364=CARTESIAN_POINT('Ctrl Pts',(-1.37831354233799,-1.99679016999301,
0.124631711935621));
#36365=CARTESIAN_POINT('Ctrl Pts',(-1.37045488139521,-1.99568051274521,
0.0016957024119192));
#36366=CARTESIAN_POINT('Origin',(-13.1285451186048,0.,0.));
#36367=CARTESIAN_POINT('',(-3.12854511860476,-1.99466715620669,0.00180221963998484));
#36368=CARTESIAN_POINT('',(-2.97045488139521,-1.99170761960215,-0.000642475566254852));
#36369=CARTESIAN_POINT('',(-13.1285451186048,-1.99475,-1.92374832954336E-13));
#36370=CARTESIAN_POINT('Ctrl Pts',(-3.12854511860476,-1.99466715620669,
0.00180221963998481));
#36371=CARTESIAN_POINT('Ctrl Pts',(-3.0963149649122,-1.99007828916401,-0.503043314735463));
#36372=CARTESIAN_POINT('Ctrl Pts',(-3.02184145169771,-1.53956787264023,
-1.67686981490333));
#36373=CARTESIAN_POINT('Ctrl Pts',(-2.90512457896129,0.430917811620456,
-2.31616994743447));
#36374=CARTESIAN_POINT('Ctrl Pts',(-2.77839450039551,2.1776462264151,-0.898994044122268));
#36375=CARTESIAN_POINT('Ctrl Pts',(-2.65166442182973,1.93932502198757,1.33766656674925));
#36376=CARTESIAN_POINT('Ctrl Pts',(-2.52493434326395,-0.066802341895476,
2.35496727045807));
#36377=CARTESIAN_POINT('Ctrl Pts',(-2.41722790885563,-1.72003362343411,
1.39511405581719));
#36378=CARTESIAN_POINT('Ctrl Pts',(-2.35176483396923,-1.99077225295041,
0.36457621733391));
#36379=CARTESIAN_POINT('Ctrl Pts',(-2.32854511860476,-1.99164273144438,
-0.000528815569653777));
#36380=CARTESIAN_POINT('Ctrl Pts',(-2.97045488139521,-1.99170761960215,
-0.000642475566254921));
#36381=CARTESIAN_POINT('Ctrl Pts',(-2.95190052326778,-1.99255428136185,
-0.292365977327294));
#36382=CARTESIAN_POINT('Ctrl Pts',(-2.89110280561841,-1.79608386950908,
-1.24718110513933));
#36383=CARTESIAN_POINT('Ctrl Pts',(-2.78806172844712,-0.324747614573964,
-2.33342489664845));
#36384=CARTESIAN_POINT('Ctrl Pts',(-2.66133164988135,1.78087291120639,-1.54234379652064));
#36385=CARTESIAN_POINT('Ctrl Pts',(-2.53460157131557,2.26312549748712,0.654672245331693));
#36386=CARTESIAN_POINT('Ctrl Pts',(-2.40787149274979,0.682409168923879,
2.25491697383304));
#36387=CARTESIAN_POINT('Ctrl Pts',(-2.28648926277634,-1.4274081023495,1.81888589547668));
#36388=CARTESIAN_POINT('Ctrl Pts',(-2.20735039232481,-1.99230096493927,
0.575003255738612));
#36389=CARTESIAN_POINT('Ctrl Pts',(-2.17045488139521,-1.99677303149338,
-0.0013452059596123));
#36390=CARTESIAN_POINT('Origin',(-13.1285451186048,0.,0.));
#36391=CARTESIAN_POINT('',(-3.92854511860476,-1.9975094432332,-0.000876183135553181));
#36392=CARTESIAN_POINT('',(-3.77045488139522,-1.99444763668832,0.00180115884744814));
#36393=CARTESIAN_POINT('',(-13.1285451186048,-1.99475,-1.92374832954336E-13));
#36394=CARTESIAN_POINT('Ctrl Pts',(-3.92854511860476,-1.9975094432332,-0.000876183135553477));
#36395=CARTESIAN_POINT('Ctrl Pts',(-3.92535181489901,-1.99778430699875,
-0.0507107092389343));
#36396=CARTESIAN_POINT('Ctrl Pts',(-3.87991515167134,-1.97353675729167,
-0.759520997005793));
#36397=CARTESIAN_POINT('Ctrl Pts',(-3.79223512892175,-1.12994078260249,
-2.06726079904157));
#36398=CARTESIAN_POINT('Ctrl Pts',(-3.66550505035595,1.11937349904418,-2.07300177355078));
#36399=CARTESIAN_POINT('Ctrl Pts',(-3.53877497179019,2.34831453822241,-0.189082555904491));
#36400=CARTESIAN_POINT('Ctrl Pts',(-3.4120448932244,1.43663198605998,1.86719627250164));
#36401=CARTESIAN_POINT('Ctrl Pts',(-3.28531481465863,-0.784623143241175,
2.22141844480153));
#36402=CARTESIAN_POINT('Ctrl Pts',(-3.19081488978541,-1.90763475622866,
0.9755918462161));
#36403=CARTESIAN_POINT('Ctrl Pts',(-3.13855832443412,-1.99609281711604,
0.158646716751444));
#36404=CARTESIAN_POINT('Ctrl Pts',(-3.12854511860476,-1.99466715620669,
0.00180221963998481));
#36405=CARTESIAN_POINT('Ctrl Pts',(-3.77045488139522,-1.99444763668832,
0.00180115884744803));
#36406=CARTESIAN_POINT('Ctrl Pts',(-3.73869401373267,-1.98997257542647,
-0.495833382664432));
#36407=CARTESIAN_POINT('Ctrl Pts',(-3.66468978654819,-1.55012106057463,
-1.6624019998815));
#36408=CARTESIAN_POINT('Ctrl Pts',(-3.5484421998418,0.405281400923077,-2.3207929105089));
#36409=CARTESIAN_POINT('Ctrl Pts',(-3.42171212127601,2.16757274388305,-0.923017413918032));
#36410=CARTESIAN_POINT('Ctrl Pts',(-3.29498204271024,1.95399702329888,1.3161414741343));
#36411=CARTESIAN_POINT('Ctrl Pts',(-3.16825196414445,-0.0407592243607493,
2.35556180878339));
#36412=CARTESIAN_POINT('Ctrl Pts',(-3.06007624370612,-1.71175158280605,
1.40994496059256));
#36413=CARTESIAN_POINT('Ctrl Pts',(-2.9941438827897,-1.99062665676483,0.371811176161177));
#36414=CARTESIAN_POINT('Ctrl Pts',(-2.97045488139521,-1.99170761960215,
-0.000642475566254921));
#36415=CARTESIAN_POINT('Origin',(-13.1285451186048,0.,0.));
#36416=CARTESIAN_POINT('',(-4.72854511860476,-1.99216358252544,-0.00112138763685431));
#36417=CARTESIAN_POINT('',(-4.57045488139521,-1.99763259114031,-0.000757564774075681));
#36418=CARTESIAN_POINT('',(-13.1285451186048,-1.99475,-1.92374832954336E-13));
#36419=CARTESIAN_POINT('Ctrl Pts',(-4.72854511860476,-1.99216358252544,
-0.00112138763685429));
#36420=CARTESIAN_POINT('Ctrl Pts',(-4.71214530536391,-1.99348757518324,
-0.258822092703375));
#36421=CARTESIAN_POINT('Ctrl Pts',(-4.65350213260112,-1.82748356051783,
-1.17867969093914));
#36422=CARTESIAN_POINT('Ctrl Pts',(-4.55261560031641,-0.442735343327605,
-2.31394010277285));
#36423=CARTESIAN_POINT('Ctrl Pts',(-4.42588552175063,1.70031488024139,-1.63072459093592));
#36424=CARTESIAN_POINT('Ctrl Pts',(-4.29915544318485,2.29343042248776,0.538990056177979));
#36425=CARTESIAN_POINT('Ctrl Pts',(-4.17242536461907,0.795952397437793,
2.21738430689477));
#36426=CARTESIAN_POINT('Ctrl Pts',(-4.04888858975905,-1.37106665451409,
1.88314514530358));
#36427=CARTESIAN_POINT('Ctrl Pts',(-3.96759517442094,-1.99414820785581,
0.608536890354887));
#36428=CARTESIAN_POINT('Ctrl Pts',(-3.92854511860476,-1.9975094432332,-0.000876183135553477));
#36429=CARTESIAN_POINT('Ctrl Pts',(-4.57045488139521,-1.99763259114031,
-0.000757564774075889));
#36430=CARTESIAN_POINT('Ctrl Pts',(-4.56773086371948,-1.99783974582131,
-0.0432614731215861));
#36431=CARTESIAN_POINT('Ctrl Pts',(-4.52276348652182,-1.97737659900053,
-0.744701853234392));
#36432=CARTESIAN_POINT('Ctrl Pts',(-4.43555274980225,-1.15272948149133,
-2.05464047695385));
#36433=CARTESIAN_POINT('Ctrl Pts',(-4.30882267123646,1.09638368952585,-2.08525191580977));
#36434=CARTESIAN_POINT('Ctrl Pts',(-4.18209259267069,2.34608015003573,-0.215036454205511));
#36435=CARTESIAN_POINT('Ctrl Pts',(-4.0553625141049,1.45718979233537,1.85119708733083));
#36436=CARTESIAN_POINT('Ctrl Pts',(-3.92863243553913,-0.760012763696535,
2.22995814895977));
#36437=CARTESIAN_POINT('Ctrl Pts',(-3.8336632246359,-1.90237578262565,0.990500269268093));
#36438=CARTESIAN_POINT('Ctrl Pts',(-3.78093737325459,-1.99592460494202,
0.166042579635038));
#36439=CARTESIAN_POINT('Ctrl Pts',(-3.77045488139522,-1.99444763668832,
0.00180115884744803));
#36440=CARTESIAN_POINT('Origin',(-13.1285451186048,0.,0.));
#36441=CARTESIAN_POINT('',(-5.52854511860476,-1.99348645498109,0.0016885444496981));
#36442=CARTESIAN_POINT('',(-5.37045488139522,-1.99229499213755,-0.00121350091589825));
#36443=CARTESIAN_POINT('',(-13.1285451186048,-1.99475,-1.92374832954336E-13));
#36444=CARTESIAN_POINT('Ctrl Pts',(-5.52854511860476,-1.99348645498109,
0.00168854444969823));
#36445=CARTESIAN_POINT('Ctrl Pts',(-5.49893879582879,-1.98972409259997,
-0.462757055610613));
#36446=CARTESIAN_POINT('Ctrl Pts',(-5.42708911353091,-1.59690446533444,
-1.59562792885432));
#36447=CARTESIAN_POINT('Ctrl Pts',(-5.31299607171107,0.286994225274642,
-2.33836859757207));
#36448=CARTESIAN_POINT('Ctrl Pts',(-5.18626599314531,2.11794332300315,-1.03181852280261));
#36449=CARTESIAN_POINT('Ctrl Pts',(-5.05953591457952,2.01826542478903,1.21529340430752));
#36450=CARTESIAN_POINT('Ctrl Pts',(-4.93280583601374,0.0788226604640474,
2.35459558558354));
#36451=CARTESIAN_POINT('Ctrl Pts',(-4.82247557068882,-1.67219508841024,
1.47786799290997));
#36452=CARTESIAN_POINT('Ctrl Pts',(-4.75438866488583,-1.99007717672159,
0.404974706278286));
#36453=CARTESIAN_POINT('Ctrl Pts',(-4.72854511860476,-1.99216358252544,
-0.00112138763685429));
#36454=CARTESIAN_POINT('Ctrl Pts',(-5.37045488139522,-1.99229499213755,
-0.00121350091589837));
#36455=CARTESIAN_POINT('Ctrl Pts',(-5.35452435418437,-1.99369239809736,
-0.251498549257047));
#36456=CARTESIAN_POINT('Ctrl Pts',(-5.2963504674516,-1.83402193695601,-1.16375266509536));
#36457=CARTESIAN_POINT('Ctrl Pts',(-5.19593322119692,-0.468293640578219,
-2.30890316237654));
#36458=CARTESIAN_POINT('Ctrl Pts',(-5.06920314263113,1.68217981160309,-1.64942530248376));
#36459=CARTESIAN_POINT('Ctrl Pts',(-4.94247306406536,2.29924973922467,0.513598465451003));
#36460=CARTESIAN_POINT('Ctrl Pts',(-4.81574298549957,0.820421458075195,
2.20844773045863));
#36461=CARTESIAN_POINT('Ctrl Pts',(-4.69173692460954,-1.3584062128533,1.89701129862388));
#36462=CARTESIAN_POINT('Ctrl Pts',(-4.60997422324141,-1.99462724476305,
0.61587811228097));
#36463=CARTESIAN_POINT('Ctrl Pts',(-4.57045488139521,-1.99763259114031,
-0.000757564774075889));
#36464=CARTESIAN_POINT('Origin',(-13.1285451186048,0.,0.));
#36465=CARTESIAN_POINT('',(-6.32854511860476,-1.9979722269169,-0.000164116242219921));
#36466=CARTESIAN_POINT('',(-6.17045488139522,-1.99329205388752,0.00164168227339369));
#36467=CARTESIAN_POINT('',(-13.1285451186048,-1.99475,-1.92374832954336E-13));
#36468=CARTESIAN_POINT('Ctrl Pts',(-6.32854511860477,-1.9979722269169,-0.000164116242220302));
#36469=CARTESIAN_POINT('Ctrl Pts',(-6.32797564581561,-1.99798275077873,
-0.00904578607702301));
#36470=CARTESIAN_POINT('Ctrl Pts',(-6.28516281350453,-1.99391352194935,
-0.676757756073187));
#36471=CARTESIAN_POINT('Ctrl Pts',(-6.20010662167154,-1.25550409505514,
-1.9935001506777));
#36472=CARTESIAN_POINT('Ctrl Pts',(-6.07337654310573,0.989158387733211,
-2.13819995964578));
#36473=CARTESIAN_POINT('Ctrl Pts',(-5.94664646453999,2.33214618174238,-0.333807684807691));
#36474=CARTESIAN_POINT('Ctrl Pts',(-5.81991638597417,1.54924877001712,1.77486946901812));
#36475=CARTESIAN_POINT('Ctrl Pts',(-5.69318630740843,-0.645877886154986,
2.26565115135322));
#36476=CARTESIAN_POINT('Ctrl Pts',(-5.59606255161859,-1.87697369462381,
1.05898945087646));
#36477=CARTESIAN_POINT('Ctrl Pts',(-5.54118215535072,-1.9950923657192,0.199930526707089));
#36478=CARTESIAN_POINT('Ctrl Pts',(-5.52854511860476,-1.99348645498109,
0.00168854444969823));
#36479=CARTESIAN_POINT('Ctrl Pts',(-6.17045488139522,-1.99329205388752,
0.00164168227339381));
#36480=CARTESIAN_POINT('Ctrl Pts',(-6.14131784464926,-1.98971745724335,
-0.455554751072749));
#36481=CARTESIAN_POINT('Ctrl Pts',(-6.06993744838138,-1.60673514178807,
-1.58101374092423));
#36482=CARTESIAN_POINT('Ctrl Pts',(-5.95631369259159,0.261121169457012,
-2.34139883016539));
#36483=CARTESIAN_POINT('Ctrl Pts',(-5.8295836140258,2.10640484398777,-1.0551736256481));
#36484=CARTESIAN_POINT('Ctrl Pts',(-5.70285353546004,2.03157950898151,1.19290294899666));
#36485=CARTESIAN_POINT('Ctrl Pts',(-5.57612345689424,0.104852755347087,
2.35357996395588));
#36486=CARTESIAN_POINT('Ctrl Pts',(-5.46532390553932,-1.66324055776191,
1.49262058419748));
#36487=CARTESIAN_POINT('Ctrl Pts',(-5.3967677137063,-1.98998686333524,0.412188291743562));
#36488=CARTESIAN_POINT('Ctrl Pts',(-5.37045488139522,-1.99229499213755,
-0.00121350091589837));
#36489=CARTESIAN_POINT('Origin',(-13.1285451186048,0.,0.));
#36490=CARTESIAN_POINT('',(-7.12854511860477,-1.99302733218635,-0.00156197182782427));
#36491=CARTESIAN_POINT('',(-6.97045488139522,-1.99798886456863,-2.89228984749754E-5));
#36492=CARTESIAN_POINT('',(-13.1285451186048,-1.99475,-1.92374832954336E-13));
#36493=CARTESIAN_POINT('Ctrl Pts',(-7.12854511860477,-1.99302733218635,
-0.00156197182782411));
#36494=CARTESIAN_POINT('Ctrl Pts',(-7.11476913628051,-1.99462045073153,
-0.217796874425585));
#36495=CARTESIAN_POINT('Ctrl Pts',(-7.05874979443432,-1.86269372181647,
-1.09521440278052));
#36496=CARTESIAN_POINT('Ctrl Pts',(-6.96048709306619,-0.584852130314656,
-2.28216593812101));
#36497=CARTESIAN_POINT('Ctrl Pts',(-6.83375701450043,1.59631522845185,-1.73266011521722));
#36498=CARTESIAN_POINT('Ctrl Pts',(-6.70702693593464,2.32234956235835,0.396264928634968));
#36499=CARTESIAN_POINT('Ctrl Pts',(-6.58029685736886,0.931428871827763,
2.16397172813741));
#36500=CARTESIAN_POINT('Ctrl Pts',(-6.45413625159224,-1.29847722763132,
1.96001463265738));
#36501=CARTESIAN_POINT('Ctrl Pts',(-6.37021900533753,-1.99720209314702,
0.649794423907979));
#36502=CARTESIAN_POINT('Ctrl Pts',(-6.32854511860477,-1.9979722269169,-0.000164116242220302));
#36503=CARTESIAN_POINT('Ctrl Pts',(-6.97045488139522,-1.99798865963142,
-2.89210683962205E-5));
#36504=CARTESIAN_POINT('Ctrl Pts',(-6.97035469463609,-1.99798899549594,
-0.00159142903403707));
#36505=CARTESIAN_POINT('Ctrl Pts',(-6.92801114835502,-1.99728097638184,
-0.661979064342672));
#36506=CARTESIAN_POINT('Ctrl Pts',(-6.84342424255203,-1.27746953458014,
-1.97949598010661));
#36507=CARTESIAN_POINT('Ctrl Pts',(-6.71669416398625,0.965455645273396,
-2.1490063154975));
#36508=CARTESIAN_POINT('Ctrl Pts',(-6.58996408542047,2.32831254761179,-0.359573952994307));
#36509=CARTESIAN_POINT('Ctrl Pts',(-6.4632340068547,1.56877882193404,1.75763072199189));
#36510=CARTESIAN_POINT('Ctrl Pts',(-6.33650392828891,-0.620786912340788,
2.27265403361463));
#36511=CARTESIAN_POINT('Ctrl Pts',(-6.23891088646909,-1.87116208516676,
1.07391421228489));
#36512=CARTESIAN_POINT('Ctrl Pts',(-6.18356120417119,-1.99489996679304,
0.207296227027028));
#36513=CARTESIAN_POINT('Ctrl Pts',(-6.17045488139522,-1.99329205388752,
0.00164168227339381));
#36514=CARTESIAN_POINT('Origin',(-13.1285451186048,0.,0.));
#36515=CARTESIAN_POINT('',(-7.92854511860477,-1.99250106198237,0.0013356187689274));
#36516=CARTESIAN_POINT('',(-7.77045488139522,-1.99321120987985,-0.00161938525380073));
#36517=CARTESIAN_POINT('',(-13.1285451186048,-1.99475,-1.92374832954336E-13));
#36518=CARTESIAN_POINT('Ctrl Pts',(-7.92854511860477,-1.99250106198237,
0.00133561876892717));
#36519=CARTESIAN_POINT('Ctrl Pts',(-7.90156262674539,-1.9898790361083,-0.422477199748252));
#36520=CARTESIAN_POINT('Ctrl Pts',(-7.83233677536409,-1.65025022702601,
-1.51364290830163));
#36521=CARTESIAN_POINT('Ctrl Pts',(-7.72086756446086,0.141974088420104,
-2.35163278207385));
#36522=CARTESIAN_POINT('Ctrl Pts',(-7.5941374858951,2.05014815624844,-1.16070061638369));
#36523=CARTESIAN_POINT('Ctrl Pts',(-7.46740740732931,2.08949441685714,1.08827683305561));
#36524=CARTESIAN_POINT('Ctrl Pts',(-7.34067732876354,0.224146493614207,
2.3452274373418));
#36525=CARTESIAN_POINT('Ctrl Pts',(-7.22772323252202,-1.62054376456912,
1.56012082295419));
#36526=CARTESIAN_POINT('Ctrl Pts',(-7.15701249580243,-1.98973523253938,
0.445276619472374));
#36527=CARTESIAN_POINT('Ctrl Pts',(-7.12854511860477,-1.99302733218635,
-0.00156197182782411));
#36528=CARTESIAN_POINT('Ctrl Pts',(-7.77045488139522,-1.99321120987985,
-0.0016193852538011));
#36529=CARTESIAN_POINT('Ctrl Pts',(-7.75714818510097,-1.99481690227094,
-0.210439444705621));
#36530=CARTESIAN_POINT('Ctrl Pts',(-7.7015981292848,-1.86864990103976,-1.08028727279676));
#36531=CARTESIAN_POINT('Ctrl Pts',(-7.6038047139467,-0.610050402621316,
-2.27555954730001));
#36532=CARTESIAN_POINT('Ctrl Pts',(-7.47707463538092,1.57705941561997,-1.75020465850163));
#36533=CARTESIAN_POINT('Ctrl Pts',(-7.35034455681515,2.32658898847186,0.370562310224418));
#36534=CARTESIAN_POINT('Ctrl Pts',(-7.22361447824936,0.955299056467363,
2.15354044767035));
#36535=CARTESIAN_POINT('Ctrl Pts',(-7.09698458644272,-1.28502834164932,
1.97358514194292));
#36536=CARTESIAN_POINT('Ctrl Pts',(-7.01259805415801,-1.99784737952166,
0.657234011746362));
#36537=CARTESIAN_POINT('Ctrl Pts',(-6.97045488139522,-1.99798865963142,
-2.89210683962205E-5));
#36538=CARTESIAN_POINT('Origin',(-13.1285451186048,0.,0.));
#36539=CARTESIAN_POINT('',(-8.72854511860477,-1.99778044304682,0.000580414400251015));
#36540=CARTESIAN_POINT('',(-8.57045488139522,-1.99235441329993,0.00125123217891654));
#36541=CARTESIAN_POINT('',(-13.1285451186048,-1.99475,-1.92374832954336E-13));
#36542=CARTESIAN_POINT('Ctrl Pts',(-8.72854511860477,-1.99778044304682,
0.000580414400251001));
#36543=CARTESIAN_POINT('Ctrl Pts',(-8.68835611721029,-1.99536078015132,
-0.626380726430122));
#36544=CARTESIAN_POINT('Ctrl Pts',(-8.60592375629387,-1.34009769434388,
-1.91671199912222));
#36545=CARTESIAN_POINT('Ctrl Pts',(-8.48124803585554,0.85516388839699,-2.19522848691248));
#36546=CARTESIAN_POINT('Ctrl Pts',(-8.35451795728975,2.30706713390257,-0.47725739709158));
#36547=CARTESIAN_POINT('Ctrl Pts',(-8.22778787872399,1.65594616616223,1.67576122332812));
#36548=CARTESIAN_POINT('Ctrl Pts',(-8.10105780015819,-0.504664851331058,
2.30122723164079));
#36549=CARTESIAN_POINT('Ctrl Pts',(-8.0013102134518,-1.8431691324066,1.14245048428309));
#36550=CARTESIAN_POINT('Ctrl Pts',(-7.94380598626732,-1.99398403805739,
0.241037399123113));
#36551=CARTESIAN_POINT('Ctrl Pts',(-7.92854511860477,-1.99250106198237,
0.00133561876892717));
#36552=CARTESIAN_POINT('Ctrl Pts',(-8.57045488139522,-1.99235441329993,
0.0012512321789164));
#36553=CARTESIAN_POINT('Ctrl Pts',(-8.54394167556586,-1.98995194175533,
-0.415267451224239));
#36554=CARTESIAN_POINT('Ctrl Pts',(-8.47518511021458,-1.65937989506407,
-1.49891452050869));
#36555=CARTESIAN_POINT('Ctrl Pts',(-8.36418518534137,0.11596324319048,-2.35305870594664));
#36556=CARTESIAN_POINT('Ctrl Pts',(-8.2374551067756,2.0371887677672,-1.1832982174768));
#36557=CARTESIAN_POINT('Ctrl Pts',(-8.11072502820981,2.10139971207879,1.06510656604636));
#36558=CARTESIAN_POINT('Ctrl Pts',(-7.98399494964405,0.250064112115891,
2.34260553378614));
#36559=CARTESIAN_POINT('Ctrl Pts',(-7.8705715673725,-1.61089390858375,1.57476690963073));
#36560=CARTESIAN_POINT('Ctrl Pts',(-7.7993915446229,-1.98971948068271,0.452479483610746));
#36561=CARTESIAN_POINT('Ctrl Pts',(-7.77045488139522,-1.99321120987985,
-0.0016193852538011));
#36562=CARTESIAN_POINT('Origin',(-13.1285451186048,0.,0.));
#36563=CARTESIAN_POINT('',(-9.52854511860476,-1.99413929912365,-0.00178482837013569));
#36564=CARTESIAN_POINT('',(-9.37045488139522,-1.99768040091508,0.000705460530160528));
#36565=CARTESIAN_POINT('',(-13.1285451186048,-1.99475,-1.92374832954336E-13));
#36566=CARTESIAN_POINT('Ctrl Pts',(-9.52854511860476,-1.99413929912365,
-0.00178482837013546));
#36567=CARTESIAN_POINT('Ctrl Pts',(-9.5173929671971,-1.99567604089445,-0.176587503202193));
#36568=CARTESIAN_POINT('Ctrl Pts',(-9.46399745626751,-1.89470323252639,
-1.0117808002804));
#36569=CARTESIAN_POINT('Ctrl Pts',(-9.368358585816,-0.724734298212267,-2.24167199518702));
#36570=CARTESIAN_POINT('Ctrl Pts',(-9.2416285072502,1.48621635193257,-1.82797549873587));
#36571=CARTESIAN_POINT('Ctrl Pts',(-9.11489842868443,2.34239544440841,0.252025761717839));
#36572=CARTESIAN_POINT('Ctrl Pts',(-8.98816835011866,1.06334653056341,2.10229101340218));
#36573=CARTESIAN_POINT('Ctrl Pts',(-8.86143827155287,-1.18500382101302,
2.03619727482286));
#36574=CARTESIAN_POINT('Ctrl Pts',(-8.77489719438158,-1.98270767494886,
0.723567688852132));
#36575=CARTESIAN_POINT('Ctrl Pts',(-8.73059947673221,-1.99790412997515,
0.03262905135474));
#36576=CARTESIAN_POINT('Ctrl Pts',(-8.72854511860477,-1.99778044304682,
0.000580414400251001));
#36577=CARTESIAN_POINT('Ctrl Pts',(-9.37045488139522,-1.99768040091508,
0.000705460530160329));
#36578=CARTESIAN_POINT('Ctrl Pts',(-9.33073516603075,-1.99484052238671,
-0.619017268744858));
#36579=CARTESIAN_POINT('Ctrl Pts',(-9.24877209114436,-1.35295791994823,
-1.90291681631474));
#36580=CARTESIAN_POINT('Ctrl Pts',(-9.12456565673604,0.830838775459797,
-2.20454977051161));
#36581=CARTESIAN_POINT('Ctrl Pts',(-8.99783557817027,2.30164890208838,-0.502737585433884));
#36582=CARTESIAN_POINT('Ctrl Pts',(-8.87110549960448,1.67437384270186,1.65734877959569));
#36583=CARTESIAN_POINT('Ctrl Pts',(-8.74437542103871,-0.479189150904811,
2.30666653572304));
#36584=CARTESIAN_POINT('Ctrl Pts',(-8.64415854830229,-1.83678140535602,
1.15737884639853));
#36585=CARTESIAN_POINT('Ctrl Pts',(-8.58618503508779,-1.99377978776735,
0.248369703929462));
#36586=CARTESIAN_POINT('Ctrl Pts',(-8.57045488139522,-1.99235441329993,
0.0012512321789164));
#36587=CARTESIAN_POINT('Origin',(-13.1285451186048,0.,0.));
#36588=CARTESIAN_POINT('',(-10.3285451186048,-1.99182186837539,0.000801948237002644));
#36589=CARTESIAN_POINT('',(-10.1704548813952,-1.99435467562299,-0.00179807465759962));
#36590=CARTESIAN_POINT('',(-13.1285451186048,-1.99475,-1.92374832954336E-13));
#36591=CARTESIAN_POINT('Ctrl Pts',(-10.3285451186048,-1.99182186837539,
0.000801948237002768));
#36592=CARTESIAN_POINT('Ctrl Pts',(-10.304186457662,-1.99043382219268,-0.38212649427497));
#36593=CARTESIAN_POINT('Ctrl Pts',(-10.2375844371973,-1.69972871911625,
-1.43109111249991));
#36594=CARTESIAN_POINT('Ctrl Pts',(-10.1287390572107,-0.00358806096914,
-2.35590932209698));
#36595=CARTESIAN_POINT('Ctrl Pts',(-10.0020089786449,1.97451952674142,-1.2851492017786));
#36596=CARTESIAN_POINT('Ctrl Pts',(-9.8752789000791,2.15273996627044,0.957102848135853));
#36597=CARTESIAN_POINT('Ctrl Pts',(-9.74854882151332,0.368613841216539,
2.32689825630081));
#36598=CARTESIAN_POINT('Ctrl Pts',(-9.63297089435521,-1.56495415031113,
1.64170776389411));
#36599=CARTESIAN_POINT('Ctrl Pts',(-9.55963632671902,-1.9898549994879,0.485549511297817));
#36600=CARTESIAN_POINT('Ctrl Pts',(-9.52854511860476,-1.99413929912365,
-0.00178482837013546));
#36601=CARTESIAN_POINT('Ctrl Pts',(-10.1704548813952,-1.99435467562299,
-0.00179807465759959));
#36602=CARTESIAN_POINT('Ctrl Pts',(-10.1597720160176,-1.99585127079878,
-0.16919896214573));
#36603=CARTESIAN_POINT('Ctrl Pts',(-10.106845791118,-1.90010097116099,-0.996867385757571));
#36604=CARTESIAN_POINT('Ctrl Pts',(-10.0116762066965,-0.749476153859556,
-2.23352110175442));
#36605=CARTESIAN_POINT('Ctrl Pts',(-9.88494612813071,1.46591330801472,-1.84429699356347));
#36606=CARTESIAN_POINT('Ctrl Pts',(-9.75821604956493,2.34503881318019,0.22611040137808));
#36607=CARTESIAN_POINT('Ctrl Pts',(-9.63148597099915,1.08652661928962,2.09040484243106));
#36608=CARTESIAN_POINT('Ctrl Pts',(-9.50475589243338,-1.16241693685793,
2.04917537014711));
#36609=CARTESIAN_POINT('Ctrl Pts',(-9.41774552923206,-1.97898996654308,
0.738376615426936));
#36610=CARTESIAN_POINT('Ctrl Pts',(-9.37297852555267,-1.99786083631826,
0.0400803561110824));
#36611=CARTESIAN_POINT('Ctrl Pts',(-9.37045488139522,-1.99768040091508,
0.000705460530160329));
#36612=CARTESIAN_POINT('Origin',(-13.1285451186048,0.,0.));
#36613=CARTESIAN_POINT('',(-11.1285451186048,-1.99700380788516,0.00135048458759499));
#36614=CARTESIAN_POINT('',(-10.9704548813952,-1.99173416440345,0.000704422997178239));
#36615=CARTESIAN_POINT('',(-13.1285451186048,-1.99475,-1.92374832954336E-13));
#36616=CARTESIAN_POINT('Ctrl Pts',(-11.1285451186048,-1.99700380788516,
0.00135048458759495));
#36617=CARTESIAN_POINT('Ctrl Pts',(-11.0909799481269,-1.99278503355486,
-0.585230740927899));
#36618=CARTESIAN_POINT('Ctrl Pts',(-11.0111714181271,-1.41024709685789,
-1.8391755479592));
#36619=CARTESIAN_POINT('Ctrl Pts',(-10.8891195286053,0.717923294984202,
-2.24374937306581));
#36620=CARTESIAN_POINT('Ctrl Pts',(-10.7623894500395,2.27316203258867,-0.618946575035767));
#36621=CARTESIAN_POINT('Ctrl Pts',(-10.6356593714738,1.75632236943564,1.57028323687515));
#36622=CARTESIAN_POINT('Ctrl Pts',(-10.508929292908,-0.361526663326025,
2.32799343505198));
#36623=CARTESIAN_POINT('Ctrl Pts',(-10.406557875285,-1.80608791742609,1.22590108173666));
#36624=CARTESIAN_POINT('Ctrl Pts',(-10.3464298171839,-1.99284100434719,
0.281956966889221));
#36625=CARTESIAN_POINT('Ctrl Pts',(-10.3285451186048,-1.99182186837539,
0.000801948237002768));
#36626=CARTESIAN_POINT('Ctrl Pts',(-10.9704548813952,-1.99173416440345,
0.000704422997178135));
#36627=CARTESIAN_POINT('Ctrl Pts',(-10.9465655064825,-1.99056444425807,
-0.37489151711618));
#36628=CARTESIAN_POINT('Ctrl Pts',(-10.8804327720478,-1.70818809927551,
-1.41629846064639));
#36629=CARTESIAN_POINT('Ctrl Pts',(-10.7720566780912,-0.0296318476642994,
-2.35571138038688));
#36630=CARTESIAN_POINT('Ctrl Pts',(-10.6453265995254,1.96018587726147,-1.30691036088261));
#36631=CARTESIAN_POINT('Ctrl Pts',(-10.5185965209596,2.16319248849083,0.933245180944391));
#36632=CARTESIAN_POINT('Ctrl Pts',(-10.3918664423938,0.394319168136422,
2.32267805209636));
#36633=CARTESIAN_POINT('Ctrl Pts',(-10.2758192292057,-1.5545868425617,1.65621678803195));
#36634=CARTESIAN_POINT('Ctrl Pts',(-10.2020153755395,-1.98993326979109,
0.492756011961213));
#36635=CARTESIAN_POINT('Ctrl Pts',(-10.1704548813952,-1.99435467562299,
-0.00179807465759959));
#36636=CARTESIAN_POINT('Ctrl Pts',(-11.9126273851832,-0.875140871775474,
1.79252782880715));
#36637=CARTESIAN_POINT('Ctrl Pts',(-11.8703840256612,-1.46986319122015,
1.50217484195868));
#36638=CARTESIAN_POINT('Ctrl Pts',(-11.7858973066174,-2.33753098893177,
0.288226582968726));
#36639=CARTESIAN_POINT('Ctrl Pts',(-11.6591672280516,-1.51239476231416,
-1.80838669328082));
#36640=CARTESIAN_POINT('Ctrl Pts',(-11.5324371494858,0.693331691078553,
-2.2508689680574));
#36641=CARTESIAN_POINT('Ctrl Pts',(-11.4057070709201,2.2660422239822,-0.644398977329155));
#36642=CARTESIAN_POINT('Ctrl Pts',(-11.2789769923543,1.77364945549679,1.55095382729707));
#36643=CARTESIAN_POINT('Ctrl Pts',(-11.1522469137885,-0.335801440579385,
2.33175063016555));
#36644=CARTESIAN_POINT('Ctrl Pts',(-11.0255168352227,-2.13900593722502,
0.987427802354548));
#36645=CARTESIAN_POINT('Ctrl Pts',(-10.898786756657,-1.99245923770595,-1.25720460847756));
#36646=CARTESIAN_POINT('Ctrl Pts',(-10.7720566780912,-0.0296318476642994,
-2.35571138038688));
#36647=CARTESIAN_POINT('Ctrl Pts',(-10.6453265995254,1.96018587726147,-1.30691036088261));
#36648=CARTESIAN_POINT('Ctrl Pts',(-10.5185965209596,2.16319248849083,0.933245180944391));
#36649=CARTESIAN_POINT('Ctrl Pts',(-10.3918664423938,0.394319168136422,
2.32267805209636));
#36650=CARTESIAN_POINT('Ctrl Pts',(-10.265136363828,-1.73399572256841,1.59486489712634));
#36651=CARTESIAN_POINT('Ctrl Pts',(-10.1384062852623,-2.28167548395771,
-0.586763647263183));
#36652=CARTESIAN_POINT('Ctrl Pts',(-10.0116762066965,-0.749476153859556,
-2.23352110175442));
#36653=CARTESIAN_POINT('Ctrl Pts',(-9.88494612813071,1.46591330801472,-1.84429699356347));
#36654=CARTESIAN_POINT('Ctrl Pts',(-9.75821604956493,2.34503881318019,0.22611040137808));
#36655=CARTESIAN_POINT('Ctrl Pts',(-9.63148597099915,1.08652661928962,2.09040484243106));
#36656=CARTESIAN_POINT('Ctrl Pts',(-9.50475589243338,-1.16241693685793,
2.04917537014711));
#36657=CARTESIAN_POINT('Ctrl Pts',(-9.37802581386759,-2.35175071733265,
0.140004748881306));
#36658=CARTESIAN_POINT('Ctrl Pts',(-9.25129573530182,-1.39732861457205,
-1.89678819466818));
#36659=CARTESIAN_POINT('Ctrl Pts',(-9.12456565673604,0.830838775459797,
-2.20454977051161));
#36660=CARTESIAN_POINT('Ctrl Pts',(-8.99783557817027,2.30164890208838,-0.502737585433884));
#36661=CARTESIAN_POINT('Ctrl Pts',(-8.87110549960448,1.67437384270186,1.65734877959569));
#36662=CARTESIAN_POINT('Ctrl Pts',(-8.74437542103871,-0.479189150904811,
2.30666653572304));
#36663=CARTESIAN_POINT('Ctrl Pts',(-8.61764534247293,-2.195943708986,0.853325245121742));
#36664=CARTESIAN_POINT('Ctrl Pts',(-8.49091526390715,-1.91096943851369,
-1.37787102135406));
#36665=CARTESIAN_POINT('Ctrl Pts',(-8.36418518534137,0.11596324319048,-2.35305870594664));
#36666=CARTESIAN_POINT('Ctrl Pts',(-8.2374551067756,2.0371887677672,-1.1832982174768));
#36667=CARTESIAN_POINT('Ctrl Pts',(-8.11072502820981,2.10139971207879,1.06510656604636));
#36668=CARTESIAN_POINT('Ctrl Pts',(-7.98399494964405,0.250064112115891,
2.34260553378614));
#36669=CARTESIAN_POINT('Ctrl Pts',(-7.85726487107825,-1.82921929001621,
1.48468499556677));
#36670=CARTESIAN_POINT('Ctrl Pts',(-7.73053479251248,-2.24106423689609,
-0.726611198051787));
#36671=CARTESIAN_POINT('Ctrl Pts',(-7.6038047139467,-0.610050402621316,
-2.27555954730001));
#36672=CARTESIAN_POINT('Ctrl Pts',(-7.47707463538092,1.57705941561997,-1.75020465850163));
#36673=CARTESIAN_POINT('Ctrl Pts',(-7.35034455681515,2.32658898847186,0.370562310224418));
#36674=CARTESIAN_POINT('Ctrl Pts',(-7.22361447824936,0.955299056467363,
2.15354044767035));
#36675=CARTESIAN_POINT('Ctrl Pts',(-7.09688439968359,-1.28680083895008,
1.97344276530014));
#36676=CARTESIAN_POINT('Ctrl Pts',(-6.97015432111781,-2.35590785438983,
-0.005561354392871));
#36677=CARTESIAN_POINT('Ctrl Pts',(-6.84342424255203,-1.27746953458014,
-1.97949598010661));
#36678=CARTESIAN_POINT('Ctrl Pts',(-6.71669416398625,0.965455645273396,
-2.1490063154975));
#36679=CARTESIAN_POINT('Ctrl Pts',(-6.58996408542047,2.32831254761179,-0.359573952994307));
#36680=CARTESIAN_POINT('Ctrl Pts',(-6.4632340068547,1.56877882193404,1.75763072199189));
#36681=CARTESIAN_POINT('Ctrl Pts',(-6.33650392828891,-0.620786912340788,
2.27265403361463));
#36682=CARTESIAN_POINT('Ctrl Pts',(-6.20977384972314,-2.24446971732477,
0.716022649816709));
#36683=CARTESIAN_POINT('Ctrl Pts',(-6.08304377115735,-1.82218945012484,
-1.49330450842827));
#36684=CARTESIAN_POINT('Ctrl Pts',(-5.95631369259159,0.261121169457012,
-2.34139883016539));
#36685=CARTESIAN_POINT('Ctrl Pts',(-5.8295836140258,2.10640484398777,-1.0551736256481));
#36686=CARTESIAN_POINT('Ctrl Pts',(-5.70285353546004,2.03157950898151,1.19290294899666));
#36687=CARTESIAN_POINT('Ctrl Pts',(-5.57612345689424,0.104852755347087,
2.35357996395588));
#36688=CARTESIAN_POINT('Ctrl Pts',(-5.44939337832848,-1.91745330764535,
1.36883364951275));
#36689=CARTESIAN_POINT('Ctrl Pts',(-5.32266329976268,-2.19189054006374,
-0.863683163791881));
#36690=CARTESIAN_POINT('Ctrl Pts',(-5.19593322119692,-0.468293640578219,
-2.30890316237654));
#36691=CARTESIAN_POINT('Ctrl Pts',(-5.06920314263113,1.68217981160309,-1.64942530248376));
#36692=CARTESIAN_POINT('Ctrl Pts',(-4.94247306406536,2.29924973922467,0.513598465451003));
#36693=CARTESIAN_POINT('Ctrl Pts',(-4.81574298549957,0.820421458075195,
2.20844773045863));
#36694=CARTESIAN_POINT('Ctrl Pts',(-4.68901290693381,-1.40626810803312,
1.89017003345429));
#36695=CARTESIAN_POINT('Ctrl Pts',(-4.56228282836801,-2.35106351606113,
-0.151106222517994));
#36696=CARTESIAN_POINT('Ctrl Pts',(-4.43555274980225,-1.15272948149133,
-2.05464047695385));
#36697=CARTESIAN_POINT('Ctrl Pts',(-4.30882267123646,1.09638368952585,-2.08525191580977));
#36698=CARTESIAN_POINT('Ctrl Pts',(-4.18209259267069,2.34608015003573,-0.215036454205511));
#36699=CARTESIAN_POINT('Ctrl Pts',(-4.0553625141049,1.45718979233537,1.85119708733083));
#36700=CARTESIAN_POINT('Ctrl Pts',(-3.92863243553913,-0.760012763696535,
2.22995814895977));
#36701=CARTESIAN_POINT('Ctrl Pts',(-3.80190235697335,-2.28442002961604,
0.575984266494282));
#36702=CARTESIAN_POINT('Ctrl Pts',(-3.67517227840757,-1.72644721895094,
-1.60303235999064));
#36703=CARTESIAN_POINT('Ctrl Pts',(-3.5484421998418,0.405281400923077,-2.3207929105089));
#36704=CARTESIAN_POINT('Ctrl Pts',(-3.42171212127601,2.16757274388305,-0.923017413918032));
#36705=CARTESIAN_POINT('Ctrl Pts',(-3.29498204271024,1.95399702329888,1.3161414741343));
#36706=CARTESIAN_POINT('Ctrl Pts',(-3.16825196414445,-0.0407592243607493,
2.35556180878339));
#36707=CARTESIAN_POINT('Ctrl Pts',(-3.04152188557869,-1.99836109667082,
1.24775224690805));
#36708=CARTESIAN_POINT('Ctrl Pts',(-2.9147918070129,-2.13434204335348,-0.997455157020213));
#36709=CARTESIAN_POINT('Ctrl Pts',(-2.78806172844712,-0.324747614573964,
-2.33342489664845));
#36710=CARTESIAN_POINT('Ctrl Pts',(-2.66133164988135,1.78087291120639,-1.54234379652064));
#36711=CARTESIAN_POINT('Ctrl Pts',(-2.53460157131557,2.26312549748712,0.654672245331693));
#36712=CARTESIAN_POINT('Ctrl Pts',(-2.40787149274979,0.682409168923879,
2.25491697383304));
#36713=CARTESIAN_POINT('Ctrl Pts',(-2.28114141418401,-1.520362263158,1.79967527305601));
#36714=CARTESIAN_POINT('Ctrl Pts',(-2.15441133561823,-2.33723626077076,
-0.296073656834323));
#36715=CARTESIAN_POINT('Ctrl Pts',(-2.02768125705245,-1.02358496316198,
-2.12193474222715));
#36716=CARTESIAN_POINT('Ctrl Pts',(-1.90095117848668,1.22312246187489,-2.01352985089457));
#36717=CARTESIAN_POINT('Ctrl Pts',(-1.77422109992089,2.35488419618976,-0.0696779332279315));
#36718=CARTESIAN_POINT('Ctrl Pts',(-1.64749102135512,1.34003240157303,1.9376915050404));
#36719=CARTESIAN_POINT('Ctrl Pts',(-1.52076094278934,-0.896333389432558,
2.17873986401275));
#36720=CARTESIAN_POINT('Ctrl Pts',(-1.39403086422356,-2.31564459579178,
0.43374925475368));
#36721=CARTESIAN_POINT('Ctrl Pts',(-1.26730078565778,-1.6241036154426,-1.7066431411118));
#36722=CARTESIAN_POINT('Ctrl Pts',(-1.14057070709201,0.54788370586334,-2.29130478089007));
#36723=CARTESIAN_POINT('Ctrl Pts',(-1.01384062852623,2.22047671979483,-0.787362926702919));
#36724=CARTESIAN_POINT('Ctrl Pts',(-0.887110549960448,1.86891443749856,
1.43440541328318));
#36725=CARTESIAN_POINT('Ctrl Pts',(-0.760380471394668,-0.186150183504844,
2.34844027344827));
#36726=CARTESIAN_POINT('Ctrl Pts',(-0.633650392828891,-2.0717580026336,
1.12210023790887));
#36727=CARTESIAN_POINT('Ctrl Pts',(-0.506920314263113,-2.06840119353109,
-1.12779160550707));
#36728=CARTESIAN_POINT('Ctrl Pts',(-0.380190235697333,-0.180414554165581,
-2.34831227349832));
#36729=CARTESIAN_POINT('Ctrl Pts',(-0.253460157131555,1.87363647225322,
-1.43076438289222));
#36730=CARTESIAN_POINT('Ctrl Pts',(-0.126730078565778,2.21660082027165,
0.796119646106798));
#36731=CARTESIAN_POINT('Ctrl Pts',(-0.0422433595219261,1.10280973225228,
1.78908852524606));
#36732=CARTESIAN_POINT('Ctrl Pts',(0.,0.458732584425967,1.94128616604711));
#36733=CARTESIAN_POINT('Ctrl Pts',(-11.8249182567888,-0.94179006796741,
1.92904360906013));
#36734=CARTESIAN_POINT('Ctrl Pts',(-11.7826748972669,-1.58180539774536,
1.61657784721794));
#36735=CARTESIAN_POINT('Ctrl Pts',(-11.698188178223,-2.51555325541557,0.31017741476688));
#36736=CARTESIAN_POINT('Ctrl Pts',(-11.5714580996572,-1.62757609880992,
-1.94611025687904));
#36737=CARTESIAN_POINT('Ctrl Pts',(-11.4447280210914,0.746134618464435,
-2.42229120679946));
#36738=CARTESIAN_POINT('Ctrl Pts',(-11.3179979425257,2.43862003132311,-0.693475274930001));
#36739=CARTESIAN_POINT('Ctrl Pts',(-11.1912678639599,1.90872749189947,1.66907175465481));
#36740=CARTESIAN_POINT('Ctrl Pts',(-11.0645377853941,-0.36137549021701,
2.50933267464865));
#36741=CARTESIAN_POINT('Ctrl Pts',(-10.9378077068283,-2.30190888344055,
1.06262857453539));
#36742=CARTESIAN_POINT('Ctrl Pts',(-10.8110776282626,-2.14420144392804,
-1.35295110976236));
#36743=CARTESIAN_POINT('Ctrl Pts',(-10.6843475496968,-0.0318885572892489,
-2.53511823364523));
#36744=CARTESIAN_POINT('Ctrl Pts',(-10.557617471131,2.10947020087126,-1.40644236522273));
#36745=CARTESIAN_POINT('Ctrl Pts',(-10.4308873925652,2.32793744009374,1.00431949956666));
#36746=CARTESIAN_POINT('Ctrl Pts',(-10.3041573139994,0.424349825424849,
2.49956914492218));
#36747=CARTESIAN_POINT('Ctrl Pts',(-10.1774272354337,-1.86605380011539,
1.71632701466244));
#36748=CARTESIAN_POINT('Ctrl Pts',(-10.0506971568679,-2.4554438930004,-0.631450539060834));
#36749=CARTESIAN_POINT('Ctrl Pts',(-9.9239670783021,-0.806554945207108,
-2.40362215737953));
#36750=CARTESIAN_POINT('Ctrl Pts',(-9.79723699973633,1.57755469835229,-1.98475542274283));
#36751=CARTESIAN_POINT('Ctrl Pts',(-9.67050692117054,2.52363286241057,0.243330573568071));
#36752=CARTESIAN_POINT('Ctrl Pts',(-9.54377684260477,1.16927458382007,2.24960641438041));
#36753=CARTESIAN_POINT('Ctrl Pts',(-9.41704676403899,-1.25094457507039,
2.20523697769101));
#36754=CARTESIAN_POINT('Ctrl Pts',(-9.29031668547321,-2.53085593342896,
0.150667265370884));
#36755=CARTESIAN_POINT('Ctrl Pts',(-9.16358660690743,-1.50374671476695,
-2.04124426179772));
#36756=CARTESIAN_POINT('Ctrl Pts',(-9.03685652834166,0.894114001580982,
-2.37244442028571));
#36757=CARTESIAN_POINT('Ctrl Pts',(-8.91012644977588,2.47693845167718,-0.541025199514446));
#36758=CARTESIAN_POINT('Ctrl Pts',(-8.78339637121009,1.80189122229186,1.78356956019488));
#36759=CARTESIAN_POINT('Ctrl Pts',(-8.65666629264432,-0.515683357451122,
2.48233821950225));
#36760=CARTESIAN_POINT('Ctrl Pts',(-8.52993621407855,-2.36318293618579,
0.918313001392679));
#36761=CARTESIAN_POINT('Ctrl Pts',(-8.40320613551275,-2.05650552433943,
-1.48280726532483));
#36762=CARTESIAN_POINT('Ctrl Pts',(-8.27647605694698,0.124794800709627,
-2.53226353616516));
#36763=CARTESIAN_POINT('Ctrl Pts',(-8.14974597838121,2.19233749666553,-1.2734161374526));
#36764=CARTESIAN_POINT('Ctrl Pts',(-8.02301589981542,2.26143863404562,1.14622321683394));
#36765=CARTESIAN_POINT('Ctrl Pts',(-7.89628582124965,0.269108556966443,
2.52101426871917));
#36766=CARTESIAN_POINT('Ctrl Pts',(-7.76955574268387,-1.96852942769843,
1.59775600475416));
#36767=CARTESIAN_POINT('Ctrl Pts',(-7.64282566411809,-2.41173976448358,
-0.781948634407555));
#36768=CARTESIAN_POINT('Ctrl Pts',(-7.51609558555232,-0.656510772925826,
-2.44886217731746));
#36769=CARTESIAN_POINT('Ctrl Pts',(-7.38936550698653,1.69716549886662,-1.88349718022318));
#36770=CARTESIAN_POINT('Ctrl Pts',(-7.26263542842076,2.50377793136296,0.398783686818758));
#36771=CARTESIAN_POINT('Ctrl Pts',(-7.13590534985498,1.02805295962734,2.31755031674763));
#36772=CARTESIAN_POINT('Ctrl Pts',(-7.00917527128919,-1.38480133731686,
2.12373671028666));
#36773=CARTESIAN_POINT('Ctrl Pts',(-6.88244519272344,-2.53532967076417,
-0.00598489740401535));
#36774=CARTESIAN_POINT('Ctrl Pts',(-6.75571511415763,-1.37475937714771,
-2.130250927332));
#36775=CARTESIAN_POINT('Ctrl Pts',(-6.62898503559187,1.03898305644994,-2.31267087300897));
#36776=CARTESIAN_POINT('Ctrl Pts',(-6.50225495702608,2.50563275374858,-0.386958475545549));
#36777=CARTESIAN_POINT('Ctrl Pts',(-6.37552487846031,1.68825426966709,1.89148879970384));
#36778=CARTESIAN_POINT('Ctrl Pts',(-6.24879479989453,-0.668064956423038,
2.44573538479814));
#36779=CARTESIAN_POINT('Ctrl Pts',(-6.12206472132875,-2.4154046003378,0.770553680882268));
#36780=CARTESIAN_POINT('Ctrl Pts',(-5.99533464276297,-1.96096420751206,
-1.60703196462012));
#36781=CARTESIAN_POINT('Ctrl Pts',(-5.8686045641972,0.281007700430807,-2.51971566466393));
#36782=CARTESIAN_POINT('Ctrl Pts',(-5.74187448563141,2.26682494803545,-1.13553380109017));
#36783=CARTESIAN_POINT('Ctrl Pts',(-5.61514440706564,2.18630104655403,1.28375234850456));
#36784=CARTESIAN_POINT('Ctrl Pts',(-5.48841432849986,0.11283815756951,2.53282449227153));
#36785=CARTESIAN_POINT('Ctrl Pts',(-5.36168424993408,-2.06348319358917,
1.47308162307093));
#36786=CARTESIAN_POINT('Ctrl Pts',(-5.2349541713683,-2.35882108501659,-0.929459761009253));
#36787=CARTESIAN_POINT('Ctrl Pts',(-5.10822409280252,-0.503958064139003,
-2.48474518372476));
#36788=CARTESIAN_POINT('Ctrl Pts',(-4.98149401423675,1.81029168011427,-1.77504264494222));
#36789=CARTESIAN_POINT('Ctrl Pts',(-4.85476393567096,2.47435657277135,0.552713225133368));
#36790=CARTESIAN_POINT('Ctrl Pts',(-4.7280338571052,0.88290331954787,2.37663924203594));
#36791=CARTESIAN_POINT('Ctrl Pts',(-4.6013037785394,-1.51336702439457,2.03412207301595));
#36792=CARTESIAN_POINT('Ctrl Pts',(-4.47457369997363,-2.53011639611208,
-0.162614207798099));
#36793=CARTESIAN_POINT('Ctrl Pts',(-4.34784362140785,-1.24051934006839,
-2.21111829746129));
#36794=CARTESIAN_POINT('Ctrl Pts',(-4.22111354284208,1.17988235126313,-2.24406104989179));
#36795=CARTESIAN_POINT('Ctrl Pts',(-4.09438346427629,2.52475350565737,-0.231413253972277));
#36796=CARTESIAN_POINT('Ctrl Pts',(-3.96765338571052,1.56816681499601,1.99218101556761));
#36797=CARTESIAN_POINT('Ctrl Pts',(-3.84092330714474,-0.817894004796855,
2.39978785633972));
#36798=CARTESIAN_POINT('Ctrl Pts',(-3.71419322857896,-2.45839745844964,
0.619850219530145));
#36799=CARTESIAN_POINT('Ctrl Pts',(-3.58746315001318,-1.85793041568185,
-1.72511649719508));
#36800=CARTESIAN_POINT('Ctrl Pts',(-3.4607330714474,0.43614692266274,-2.4975404342528));
#36801=CARTESIAN_POINT('Ctrl Pts',(-3.33400299288163,2.33265128806564,-0.993312803715125));
#36802=CARTESIAN_POINT('Ctrl Pts',(-3.20727291431584,2.1028100146292,1.41637650389352));
#36803=CARTESIAN_POINT('Ctrl Pts',(-3.08054283575007,-0.0438633755078936,
2.53495727093036));
#36804=CARTESIAN_POINT('Ctrl Pts',(-2.95381275718429,-2.15055277813595,
1.34277887288933));
#36805=CARTESIAN_POINT('Ctrl Pts',(-2.82708267861851,-2.29688979557947,
-1.07341959497182));
#36806=CARTESIAN_POINT('Ctrl Pts',(-2.70035260005274,-0.349479824181215,
-2.5111344503348));
#36807=CARTESIAN_POINT('Ctrl Pts',(-2.57362252148695,1.91650107334572,-1.6598059990129));
#36808=CARTESIAN_POINT('Ctrl Pts',(-2.44689244292118,2.43548117204613,0.704530937032375));
#36809=CARTESIAN_POINT('Ctrl Pts',(-2.3201623643554,0.734380256150712,2.42664750160584));
#36810=CARTESIAN_POINT('Ctrl Pts',(-2.19343228578962,-1.63615039056481,
1.93673539014593));
#36811=CARTESIAN_POINT('Ctrl Pts',(-2.06670220722384,-2.51523608127396,
-0.31862210803575));
#36812=CARTESIAN_POINT('Ctrl Pts',(-1.93997212865807,-1.10153940138919,
-2.2835375761278));
#36813=CARTESIAN_POINT('Ctrl Pts',(-1.81324205009228,1.31627332656126,-2.1668767581169));
#36814=CARTESIAN_POINT('Ctrl Pts',(-1.68651197152651,2.53422805254828,-0.0749844825981518));
#36815=CARTESIAN_POINT('Ctrl Pts',(-1.55978189296073,1.4420869225267,2.08526269665541));
#36816=CARTESIAN_POINT('Ctrl Pts',(-1.43305181439495,-0.964596570655569,
2.34466887650786));
#36817=CARTESIAN_POINT('Ctrl Pts',(-1.30632173582917,-2.49200003290288,
0.466782838386398));
#36818=CARTESIAN_POINT('Ctrl Pts',(-1.17959165726339,-1.74779250256096,
-1.83661809395662));
#36819=CARTESIAN_POINT('Ctrl Pts',(-1.05286157869762,0.58960956941301,-2.46580654032369));
#36820=CARTESIAN_POINT('Ctrl Pts',(-0.926131500131837,2.38958433813404,
-0.847327108320492));
#36821=CARTESIAN_POINT('Ctrl Pts',(-0.799401421566058,2.01124768809639,
1.54364721753663));
#36822=CARTESIAN_POINT('Ctrl Pts',(-0.672671343000278,-0.200327055482492,
2.52729337193581));
#36823=CARTESIAN_POINT('Ctrl Pts',(-0.5459412644345,-2.22953946391951,1.20755742693457));
#36824=CARTESIAN_POINT('Ctrl Pts',(-0.419211185868724,-2.22592700611442,
-1.21368223912194));
#36825=CARTESIAN_POINT('Ctrl Pts',(-0.292481107302943,-0.194154610657383,
-2.52715562373383));
#36826=CARTESIAN_POINT('Ctrl Pts',(-0.165751028737165,2.01632934474841,
-1.53972889264753));
#36827=CARTESIAN_POINT('Ctrl Pts',(-0.0390209501713877,2.38541325689092,
0.856750724138811));
#36828=CARTESIAN_POINT('Ctrl Pts',(0.0454657688724642,1.18679779014993,
1.92534237416295));
#36829=CARTESIAN_POINT('Ctrl Pts',(0.0877091283943902,0.493668854694124,
2.08913112074919));
#36830=CARTESIAN_POINT('Ctrl Pts',(-11.7372091283944,-1.00843926415935,
2.06555938931311));
#36831=CARTESIAN_POINT('Ctrl Pts',(-11.6949657688725,-1.69374760427058,
1.73098085247721));
#36832=CARTESIAN_POINT('Ctrl Pts',(-11.6104790498286,-2.69357552189936,
0.332128246565033));
#36833=CARTESIAN_POINT('Ctrl Pts',(-11.4837489712628,-1.74275743530568,
-2.08383382047727));
#36834=CARTESIAN_POINT('Ctrl Pts',(-11.3570188926971,0.798937545850312,
-2.59371344554152));
#36835=CARTESIAN_POINT('Ctrl Pts',(-11.2302888141313,2.61119783866403,-0.742551572530846));
#36836=CARTESIAN_POINT('Ctrl Pts',(-11.1035587355655,2.04380552830215,1.78718968201255));
#36837=CARTESIAN_POINT('Ctrl Pts',(-10.9768286569997,-0.386949539854633,
2.68691471913174));
#36838=CARTESIAN_POINT('Ctrl Pts',(-10.850098578434,-2.46481182965607,1.13782934671622));
#36839=CARTESIAN_POINT('Ctrl Pts',(-10.7233684998681,-2.29594365015013,
-1.44869761104716));
#36840=CARTESIAN_POINT('Ctrl Pts',(-10.5966384213024,-0.0341452669142003,
-2.71452508690359));
#36841=CARTESIAN_POINT('Ctrl Pts',(-10.4699083427366,2.25875452448105,-1.50597436956284));
#36842=CARTESIAN_POINT('Ctrl Pts',(-10.3431782641708,2.49268239169665,1.07539381818893));
#36843=CARTESIAN_POINT('Ctrl Pts',(-10.216448185605,0.454380482713277,2.676460237748));
#36844=CARTESIAN_POINT('Ctrl Pts',(-10.0897181070393,-1.99811187766236,
1.83778913219854));
#36845=CARTESIAN_POINT('Ctrl Pts',(-9.96298802847347,-2.6292123020431,-0.676137430858485));
#36846=CARTESIAN_POINT('Ctrl Pts',(-9.83625794990772,-0.863633736554661,
-2.57372321300464));
#36847=CARTESIAN_POINT('Ctrl Pts',(-9.70952787134193,1.68919608868986,-2.1252138519222));
#36848=CARTESIAN_POINT('Ctrl Pts',(-9.58279779277616,2.70222691164095,0.260550745758062));
#36849=CARTESIAN_POINT('Ctrl Pts',(-9.45606771421037,1.25202254835052,2.40880798632976));
#36850=CARTESIAN_POINT('Ctrl Pts',(-9.3293376356446,-1.33947221328284,2.36129858523491));
#36851=CARTESIAN_POINT('Ctrl Pts',(-9.20260755707882,-2.70996114952527,
0.161329781860462));
#36852=CARTESIAN_POINT('Ctrl Pts',(-9.07587747851304,-1.61016481496184,
-2.18570032892727));
#36853=CARTESIAN_POINT('Ctrl Pts',(-8.94914739994727,0.957389227702167,
-2.54033907005982));
#36854=CARTESIAN_POINT('Ctrl Pts',(-8.82241732138147,2.65222800126598,-0.579312813595004));
#36855=CARTESIAN_POINT('Ctrl Pts',(-8.69568724281571,1.92940860188185,1.90979034079406));
#36856=CARTESIAN_POINT('Ctrl Pts',(-8.56895716424992,-0.552177563997433,
2.65800990328147));
#36857=CARTESIAN_POINT('Ctrl Pts',(-8.44222708568415,-2.53042216338558,
0.98330075766361));
#36858=CARTESIAN_POINT('Ctrl Pts',(-8.31549700711837,-2.20204161016517,
-1.58774350929558));
#36859=CARTESIAN_POINT('Ctrl Pts',(-8.18876692855259,0.133626358228775,
-2.71146836638369));
#36860=CARTESIAN_POINT('Ctrl Pts',(-8.06203684998682,2.34748622556386,-1.36353405742839));
#36861=CARTESIAN_POINT('Ctrl Pts',(-7.93530677142103,2.42147755601244,1.22733986762151));
#36862=CARTESIAN_POINT('Ctrl Pts',(-7.80857669285527,0.288153001816996,
2.69942300365221));
#36863=CARTESIAN_POINT('Ctrl Pts',(-7.68184661428947,-2.10783956538065,
1.71082701394155));
#36864=CARTESIAN_POINT('Ctrl Pts',(-7.5551165357237,-2.58241529207107,-0.837286070763322));
#36865=CARTESIAN_POINT('Ctrl Pts',(-7.42838645715792,-0.702971143230335,
-2.62216480733491));
#36866=CARTESIAN_POINT('Ctrl Pts',(-7.30165637859214,1.81727158211326,-2.01678970194473));
#36867=CARTESIAN_POINT('Ctrl Pts',(-7.17492630002637,2.68096687425406,0.427005063413098));
#36868=CARTESIAN_POINT('Ctrl Pts',(-7.04819622146058,1.10080686278732,2.48156018582491));
#36869=CARTESIAN_POINT('Ctrl Pts',(-6.92146614289481,-1.48280183568364,
2.27403065527319));
#36870=CARTESIAN_POINT('Ctrl Pts',(-6.79473606432903,-2.71475148713851,
-0.0064084404151617));
#36871=CARTESIAN_POINT('Ctrl Pts',(-6.66800598576325,-1.47204921971528,
-2.28100587455739));
#36872=CARTESIAN_POINT('Ctrl Pts',(-6.54127590719748,1.11251046762649,-2.47633543052044));
#36873=CARTESIAN_POINT('Ctrl Pts',(-6.41454582863169,2.68295295988536,-0.414342998096788));
#36874=CARTESIAN_POINT('Ctrl Pts',(-6.28781575006593,1.80772971740014,2.02534687741579));
#36875=CARTESIAN_POINT('Ctrl Pts',(-6.16108567150013,-0.715343000505289,
2.61881673598164));
#36876=CARTESIAN_POINT('Ctrl Pts',(-6.03435559293437,-2.58633948335083,
0.825084711947826));
#36877=CARTESIAN_POINT('Ctrl Pts',(-5.90762551436857,-2.09973896489927,
-1.72075942081198));
#36878=CARTESIAN_POINT('Ctrl Pts',(-5.78089543580281,0.3008942314046,-2.69803249916247));
#36879=CARTESIAN_POINT('Ctrl Pts',(-5.65416535723702,2.42724505208314,-1.21589397653224));
#36880=CARTESIAN_POINT('Ctrl Pts',(-5.52743527867125,2.34102258412655,1.37460174801246));
#36881=CARTESIAN_POINT('Ctrl Pts',(-5.40070520010546,0.120823559791933,
2.71206902058717));
#36882=CARTESIAN_POINT('Ctrl Pts',(-5.27397512153969,-2.20951307953299,
1.5773295966291));
#36883=CARTESIAN_POINT('Ctrl Pts',(-5.14724504297391,-2.52575162996943,
-0.995236358226622));
#36884=CARTESIAN_POINT('Ctrl Pts',(-5.02051496440813,-0.539622487699786,
-2.66058720507298));
#36885=CARTESIAN_POINT('Ctrl Pts',(-4.89378488584236,1.93840354862544,-1.90065998740068));
#36886=CARTESIAN_POINT('Ctrl Pts',(-4.76705480727657,2.64946340631802,0.591827984815734));
#36887=CARTESIAN_POINT('Ctrl Pts',(-4.64032472871081,0.945385181020546,
2.54483075361324));
#36888=CARTESIAN_POINT('Ctrl Pts',(-4.51359465014501,-1.62046594075601,
2.17807411257761));
#36889=CARTESIAN_POINT('Ctrl Pts',(-4.38686457157924,-2.70916927616302,
-0.174122193078205));
#36890=CARTESIAN_POINT('Ctrl Pts',(-4.26013449301346,-1.32830919864544,
-2.36759611796874));
#36891=CARTESIAN_POINT('Ctrl Pts',(-4.13340441444769,1.26338101300041,-2.40287018397382));
#36892=CARTESIAN_POINT('Ctrl Pts',(-4.00667433588191,2.70342686127901,-0.247790053739041));
#36893=CARTESIAN_POINT('Ctrl Pts',(-3.87994425731612,1.67914383765664,2.13316494380439));
#36894=CARTESIAN_POINT('Ctrl Pts',(-3.75321417875035,-0.875775245897177,
2.56961756371967));
#36895=CARTESIAN_POINT('Ctrl Pts',(-3.62648410018457,-2.63237488728325,
0.663716172566008));
#36896=CARTESIAN_POINT('Ctrl Pts',(-3.49975402161879,-1.98941361241277,
-1.84720063439951));
#36897=CARTESIAN_POINT('Ctrl Pts',(-3.37302394305301,0.467012444402406,
-2.6742879579967));
#36898=CARTESIAN_POINT('Ctrl Pts',(-3.24629386448724,2.49772983224823,-1.06360819351221));
#36899=CARTESIAN_POINT('Ctrl Pts',(-3.11956378592145,2.25162300595954,1.51661153365274));
#36900=CARTESIAN_POINT('Ctrl Pts',(-2.99283370735568,-0.0469675266550418,
2.71435273307734));
#36901=CARTESIAN_POINT('Ctrl Pts',(-2.8661036287899,-2.30274445960107,1.4378054988706));
#36902=CARTESIAN_POINT('Ctrl Pts',(-2.73937355022412,-2.45943754780547,
-1.14938403292342));
#36903=CARTESIAN_POINT('Ctrl Pts',(-2.61264347165834,-0.374212033788463,
-2.68884400402115));
#36904=CARTESIAN_POINT('Ctrl Pts',(-2.48591339309257,2.05212923548504,-1.77726820150518));
#36905=CARTESIAN_POINT('Ctrl Pts',(-2.35918331452679,2.60783684660515,0.754389628733061));
#36906=CARTESIAN_POINT('Ctrl Pts',(-2.23245323596101,0.786351343377539,
2.59837802937863));
#36907=CARTESIAN_POINT('Ctrl Pts',(-2.10572315739523,-1.75193851797162,
2.07379550723585));
#36908=CARTESIAN_POINT('Ctrl Pts',(-1.97899307882945,-2.69323590177716,
-0.341170559237177));
#36909=CARTESIAN_POINT('Ctrl Pts',(-1.85226300026368,-1.17949383961639,
-2.44514041002845));
#36910=CARTESIAN_POINT('Ctrl Pts',(-1.72553292169789,1.40942419124763,-2.32022366533924));
#36911=CARTESIAN_POINT('Ctrl Pts',(-1.59880284313212,2.7135719089068,-0.0802910319683703));
#36912=CARTESIAN_POINT('Ctrl Pts',(-1.47207276456634,1.54414144348037,2.23283388827042));
#36913=CARTESIAN_POINT('Ctrl Pts',(-1.34534268600056,-1.03285975187858,
2.51059788900296));
#36914=CARTESIAN_POINT('Ctrl Pts',(-1.21861260743478,-2.66835547001398,
0.499816422019115));
#36915=CARTESIAN_POINT('Ctrl Pts',(-1.091882528869,-1.87148138967931,-1.96659304680144));
#36916=CARTESIAN_POINT('Ctrl Pts',(-0.965152450303224,0.631335432962678,
-2.64030829975732));
#36917=CARTESIAN_POINT('Ctrl Pts',(-0.83842237173745,2.55869195647326,-0.907291289938061));
#36918=CARTESIAN_POINT('Ctrl Pts',(-0.711692293171666,2.15358093869421,
1.65288902179009));
#36919=CARTESIAN_POINT('Ctrl Pts',(-0.584962214605889,-0.214503927460137,
2.70614647042334));
#36920=CARTESIAN_POINT('Ctrl Pts',(-0.45823213604011,-2.38732092520542,
1.29301461596027));
#36921=CARTESIAN_POINT('Ctrl Pts',(-0.331502057474334,-2.38345281869776,
-1.2995728727368));
#36922=CARTESIAN_POINT('Ctrl Pts',(-0.204771978908552,-0.207894667149185,
-2.70599897396934));
#36923=CARTESIAN_POINT('Ctrl Pts',(-0.0780419003427751,2.1590222172436,
-1.64869340240284));
#36924=CARTESIAN_POINT('Ctrl Pts',(0.0486881782230028,2.55422569351019,
0.917381802170824));
#36925=CARTESIAN_POINT('Ctrl Pts',(0.133174897266854,1.27078584804759,2.06159622307983));
#36926=CARTESIAN_POINT('Ctrl Pts',(0.17541825678878,0.528605124962282,2.23697607545127));
#36927=CARTESIAN_POINT('Ctrl Pts',(-11.6495,-1.07508846035128,2.20207516956609));
#36928=CARTESIAN_POINT('Ctrl Pts',(-11.6072566404781,-1.8056898107958,1.84538385773647));
#36929=CARTESIAN_POINT('Ctrl Pts',(-11.5227699214342,-2.87159778838315,
0.354079078363186));
#36930=CARTESIAN_POINT('Ctrl Pts',(-11.3960398428684,-1.85793877180144,
-2.22155738407549));
#36931=CARTESIAN_POINT('Ctrl Pts',(-11.2693097643027,0.851740473236193,
-2.76513568428359));
#36932=CARTESIAN_POINT('Ctrl Pts',(-11.1425796857369,2.78377564600494,-0.791627870131692));
#36933=CARTESIAN_POINT('Ctrl Pts',(-11.0158496071711,2.17888356470483,1.90530760937029));
#36934=CARTESIAN_POINT('Ctrl Pts',(-10.8891195286053,-0.412523589492258,
2.86449676361484));
#36935=CARTESIAN_POINT('Ctrl Pts',(-10.7623894500395,-2.6277147758716,1.21303011889706));
#36936=CARTESIAN_POINT('Ctrl Pts',(-10.6356593714738,-2.44768585637222,
-1.54444411233196));
#36937=CARTESIAN_POINT('Ctrl Pts',(-10.508929292908,-0.036401976539149,
-2.89393194016194));
#36938=CARTESIAN_POINT('Ctrl Pts',(-10.3821992143422,2.40803884809083,-1.60550637390296));
#36939=CARTESIAN_POINT('Ctrl Pts',(-10.2554691357764,2.65742734329957,1.1464681368112));
#36940=CARTESIAN_POINT('Ctrl Pts',(-10.1287390572106,0.484411140001705,
2.85335133057382));
#36941=CARTESIAN_POINT('Ctrl Pts',(-10.0020089786449,-2.13016995520933,
1.95925124973464));
#36942=CARTESIAN_POINT('Ctrl Pts',(-9.87527890007908,-2.80298071108579,
-0.720824322656137));
#36943=CARTESIAN_POINT('Ctrl Pts',(-9.74854882151334,-0.920712527902214,
-2.74382426862974));
#36944=CARTESIAN_POINT('Ctrl Pts',(-9.62181874294753,1.80083747902744,-2.26567228110156));
#36945=CARTESIAN_POINT('Ctrl Pts',(-9.49508866438176,2.88082096087132,0.277770917948053));
#36946=CARTESIAN_POINT('Ctrl Pts',(-9.36835858581599,1.33477051288097,2.56800955827911));
#36947=CARTESIAN_POINT('Ctrl Pts',(-9.24162850725019,-1.4279998514953,2.51736019277881));
#36948=CARTESIAN_POINT('Ctrl Pts',(-9.11489842868444,-2.88906636562158,
0.171992298350041));
#36949=CARTESIAN_POINT('Ctrl Pts',(-8.98816835011864,-1.71658291515674,
-2.33015639605681));
#36950=CARTESIAN_POINT('Ctrl Pts',(-8.86143827155288,1.02066445382335,-2.70823371983393));
#36951=CARTESIAN_POINT('Ctrl Pts',(-8.73470819298709,2.82751755085477,-0.617600427675567));
#36952=CARTESIAN_POINT('Ctrl Pts',(-8.60797811442131,2.05692598147186,2.03601112139324));
#36953=CARTESIAN_POINT('Ctrl Pts',(-8.48124803585554,-0.588671770543746,
2.83368158706069));
#36954=CARTESIAN_POINT('Ctrl Pts',(-8.35451795728976,-2.69766139058536,
1.04828851393454));
#36955=CARTESIAN_POINT('Ctrl Pts',(-8.22778787872398,-2.34757769599091,
-1.69267975326635));
#36956=CARTESIAN_POINT('Ctrl Pts',(-8.1010578001582,0.142457915747924,-2.8906731966022));
#36957=CARTESIAN_POINT('Ctrl Pts',(-7.97432772159243,2.50263495446219,-1.45365197740418));
#36958=CARTESIAN_POINT('Ctrl Pts',(-7.84759764302664,2.58151647797926,1.30845651840909));
#36959=CARTESIAN_POINT('Ctrl Pts',(-7.72086756446088,0.307197446667551,
2.87783173858525));
#36960=CARTESIAN_POINT('Ctrl Pts',(-7.59413748589508,-2.24714970306288,
1.82389802312894));
#36961=CARTESIAN_POINT('Ctrl Pts',(-7.46740740732932,-2.75309081965856,
-0.892623507119088));
#36962=CARTESIAN_POINT('Ctrl Pts',(-7.34067732876353,-0.749431513534847,
-2.79546743735237));
#36963=CARTESIAN_POINT('Ctrl Pts',(-7.21394725019776,1.9373776653599,-2.15008222366628));
#36964=CARTESIAN_POINT('Ctrl Pts',(-7.08721717163197,2.85815581714516,0.455226440007436));
#36965=CARTESIAN_POINT('Ctrl Pts',(-6.9604870930662,1.1735607659473,2.6455700549022));
#36966=CARTESIAN_POINT('Ctrl Pts',(-6.83375701450042,-1.58080233405042,
2.42432460025971));
#36967=CARTESIAN_POINT('Ctrl Pts',(-6.70702693593464,-2.89417330351285,
-0.00683198342630554));
#36968=CARTESIAN_POINT('Ctrl Pts',(-6.58029685736886,-1.56933906228285,
-2.43176082178278));
#36969=CARTESIAN_POINT('Ctrl Pts',(-6.45356677880308,1.18603787880304,-2.63999998803191));
#36970=CARTESIAN_POINT('Ctrl Pts',(-6.32683670023731,2.86027316602215,-0.441727520648026));
#36971=CARTESIAN_POINT('Ctrl Pts',(-6.20010662167153,1.9272051651332,2.15920495512774));
#36972=CARTESIAN_POINT('Ctrl Pts',(-6.07337654310574,-0.762621044587542,
2.79189808716515));
#36973=CARTESIAN_POINT('Ctrl Pts',(-5.94664646453997,-2.75727436636386,
0.87961574301338));
#36974=CARTESIAN_POINT('Ctrl Pts',(-5.81991638597419,-2.23851372228649,
-1.83448687700383));
#36975=CARTESIAN_POINT('Ctrl Pts',(-5.69318630740841,0.320780762378395,
-2.87634933366101));
#36976=CARTESIAN_POINT('Ctrl Pts',(-5.56645622884264,2.58766515613083,-1.29625415197431));
#36977=CARTESIAN_POINT('Ctrl Pts',(-5.43972615027686,2.49574412169908,1.46545114752035));
#36978=CARTESIAN_POINT('Ctrl Pts',(-5.31299607171107,0.128808962014357,
2.89131354890282));
#36979=CARTESIAN_POINT('Ctrl Pts',(-5.18626599314531,-2.35554296547681,
1.68157757018728));
#36980=CARTESIAN_POINT('Ctrl Pts',(-5.05953591457952,-2.69268217492228,
-1.06101295544399));
#36981=CARTESIAN_POINT('Ctrl Pts',(-4.93280583601374,-0.575286911260571,
-2.8364292264212));
#36982=CARTESIAN_POINT('Ctrl Pts',(-4.80607575744797,2.06651541713663,-2.02627732985914));
#36983=CARTESIAN_POINT('Ctrl Pts',(-4.67934567888219,2.82457023986469,0.630942744498098));
#36984=CARTESIAN_POINT('Ctrl Pts',(-4.55261560031641,1.00786704249322,2.71302226519054));
#36985=CARTESIAN_POINT('Ctrl Pts',(-4.42588552175063,-1.72756485711747,
2.32202615213927));
#36986=CARTESIAN_POINT('Ctrl Pts',(-4.29915544318485,-2.88822215621396,
-0.18563017835831));
#36987=CARTESIAN_POINT('Ctrl Pts',(-4.17242536461907,-1.41609905722251,
-2.52407393847618));
#36988=CARTESIAN_POINT('Ctrl Pts',(-4.04569528605329,1.34687967473769,-2.56167931805584));
#36989=CARTESIAN_POINT('Ctrl Pts',(-3.91896520748752,2.88210021690064,-0.264166853505807));
#36990=CARTESIAN_POINT('Ctrl Pts',(-3.79223512892173,1.79012086031728,2.27414887204118));
#36991=CARTESIAN_POINT('Ctrl Pts',(-3.66550505035596,-0.933656486997501,
2.73944727109961));
#36992=CARTESIAN_POINT('Ctrl Pts',(-3.53877497179018,-2.80635231611685,
0.707582125601873));
#36993=CARTESIAN_POINT('Ctrl Pts',(-3.4120448932244,-2.12089680914368,-1.96928477160395));
#36994=CARTESIAN_POINT('Ctrl Pts',(-3.28531481465862,0.49787796614207,-2.85103548174061));
#36995=CARTESIAN_POINT('Ctrl Pts',(-3.15858473609284,2.66280837643082,-1.1339035833093));
#36996=CARTESIAN_POINT('Ctrl Pts',(-3.03185465752707,2.40043599728986,1.61684656341196));
#36997=CARTESIAN_POINT('Ctrl Pts',(-2.90512457896129,-0.0500716778021863,
2.89374819522431));
#36998=CARTESIAN_POINT('Ctrl Pts',(-2.77839450039551,-2.4549361410662,1.53283212485187));
#36999=CARTESIAN_POINT('Ctrl Pts',(-2.65166442182973,-2.62198530003146,
-1.22534847087502));
#37000=CARTESIAN_POINT('Ctrl Pts',(-2.52493434326395,-0.398944243395714,
-2.86655355770749));
#37001=CARTESIAN_POINT('Ctrl Pts',(-2.39820426469817,2.18775739762436,-1.89473040399744));
#37002=CARTESIAN_POINT('Ctrl Pts',(-2.2714741861324,2.78019252116416,0.804248320433746));
#37003=CARTESIAN_POINT('Ctrl Pts',(-2.14474410756662,0.838322430604369,
2.77010855715143));
#37004=CARTESIAN_POINT('Ctrl Pts',(-2.01801402900084,-1.86772664537843,
2.21085562432577));
#37005=CARTESIAN_POINT('Ctrl Pts',(-1.89128395043506,-2.87123572228036,
-0.363719010438602));
#37006=CARTESIAN_POINT('Ctrl Pts',(-1.76455387186928,-1.2574482778436,-2.60674324392911));
#37007=CARTESIAN_POINT('Ctrl Pts',(-1.6378237933035,1.50257505593399,-2.47357057256157));
#37008=CARTESIAN_POINT('Ctrl Pts',(-1.51109371473772,2.89291576526532,-0.0855975813385903));
#37009=CARTESIAN_POINT('Ctrl Pts',(-1.38436363617195,1.64619596443404,2.38040507988543));
#37010=CARTESIAN_POINT('Ctrl Pts',(-1.25763355760617,-1.10112293310158,
2.67652690149807));
#37011=CARTESIAN_POINT('Ctrl Pts',(-1.13090347904039,-2.84471090712508,
0.532850005651832));
#37012=CARTESIAN_POINT('Ctrl Pts',(-1.00417340047461,-1.99517027679767,
-2.09656799964626));
#37013=CARTESIAN_POINT('Ctrl Pts',(-0.877443321908835,0.673061296512348,
-2.81481005919094));
#37014=CARTESIAN_POINT('Ctrl Pts',(-0.750713243343059,2.72779957481248,
-0.967255471555635));
#37015=CARTESIAN_POINT('Ctrl Pts',(-0.623983164777276,2.29591418929203,
1.76213082604354));
#37016=CARTESIAN_POINT('Ctrl Pts',(-0.497253086211499,-0.228680799437782,
2.88499956891088));
#37017=CARTESIAN_POINT('Ctrl Pts',(-0.370523007645719,-2.54510238649133,
1.37847180498597));
#37018=CARTESIAN_POINT('Ctrl Pts',(-0.243792929079943,-2.5409786312811,
-1.38546350635167));
#37019=CARTESIAN_POINT('Ctrl Pts',(-0.117062850514162,-0.221634723640988,
-2.88484232420485));
#37020=CARTESIAN_POINT('Ctrl Pts',(0.0096672280516153,2.30171508973879,
-1.75765791215815));
#37021=CARTESIAN_POINT('Ctrl Pts',(0.136397306617393,2.72303813012945,0.978012880202838));
#37022=CARTESIAN_POINT('Ctrl Pts',(0.220884025661244,1.35477390594525,2.19785007199671));
#37023=CARTESIAN_POINT('Ctrl Pts',(0.263127385183171,0.563541395230439,
2.38482103015336));
#37024=CARTESIAN_POINT('',(0.,1.82956213026058,-1.63023086141699));
#37025=CARTESIAN_POINT('Ctrl Pts',(1.11022302462516E-16,1.83311928606617,
-1.63215490580859));
#37026=CARTESIAN_POINT('Ctrl Pts',(3.35691596827958E-16,1.87020221509191,
-1.58263650689979));
#37027=CARTESIAN_POINT('Ctrl Pts',(1.7799849765391E-15,1.90522161173578,
-1.53170199440537));
#37028=CARTESIAN_POINT('Ctrl Pts',(8.88178419700125E-16,1.93804364176405,
-1.47939865304506));
#37029=CARTESIAN_POINT('Ctrl Pts',(-1.77793102530655E-16,1.98336980933887,
-1.40716942124011));
#37030=CARTESIAN_POINT('Ctrl Pts',(5.39107183348623E-16,2.02450743199428,
-1.33232980239994));
#37031=CARTESIAN_POINT('Ctrl Pts',(-5.27355936696949E-16,2.06143695913673,
-1.25527886014649));
#37032=CARTESIAN_POINT('Ctrl Pts',(-1.06429201921402E-15,2.08003000305954,
-1.21648574080632));
#37033=CARTESIAN_POINT('Ctrl Pts',(2.02892540791524E-15,2.09755555354514,
-1.17713185376445));
#37034=CARTESIAN_POINT('Ctrl Pts',(1.97064586870965E-15,2.11400625054454,
-1.13726744031613));
#37035=CARTESIAN_POINT('Ctrl Pts',(1.9422168992414E-15,2.12203095988682,
-1.11782143562494));
#37036=CARTESIAN_POINT('Ctrl Pts',(4.11823233707136E-15,2.12979985614877,
-1.09825394858399));
#37037=CARTESIAN_POINT('Ctrl Pts',(4.27435864480685E-15,2.13731180430856,
-1.07857082222221));
#37038=CARTESIAN_POINT('Ctrl Pts',(4.40132187367308E-15,2.14342058384275,
-1.06256433802797));
#37039=CARTESIAN_POINT('Ctrl Pts',(-1.81383465133899E-15,2.14935611980056,
-1.04648998991835));
#37040=CARTESIAN_POINT('Ctrl Pts',(-1.52655665885959E-15,2.15511691042516,
-1.03035523241857));
#37041=CARTESIAN_POINT('Ctrl Pts',(-1.0238845684058E-16,2.18367578037281,
-0.950367871116878));
#37042=CARTESIAN_POINT('Ctrl Pts',(5.79434641801055E-15,2.20795681184397,
-0.868863550066977));
#37043=CARTESIAN_POINT('Ctrl Pts',(4.57966997657877E-15,2.22793924709077,
-0.786237832279718));
#37044=CARTESIAN_POINT('Ctrl Pts',(3.64166789715849E-15,2.24337015953301,
-0.72243228501259));
#37045=CARTESIAN_POINT('Ctrl Pts',(-2.13542367938229E-16,2.25623663051347,
-0.657957590807845));
#37046=CARTESIAN_POINT('Ctrl Pts',(-9.99200722162641E-16,2.26650784188907,
-0.592996429696028));
#37047=CARTESIAN_POINT('Ctrl Pts',(-1.39260515725901E-15,2.27165096814395,
-0.56046828466583));
#37048=CARTESIAN_POINT('Ctrl Pts',(-2.30199172467359E-16,2.276143089034,
-0.527818207731014));
#37049=CARTESIAN_POINT('Ctrl Pts',(-3.88578058618805E-16,2.27997860287735,
-0.49506956990305));
#37050=CARTESIAN_POINT('Ctrl Pts',(-4.77966372939306E-16,2.28214334923554,
-0.476586389456036));
#37051=CARTESIAN_POINT('Ctrl Pts',(1.21427467872323E-15,2.28409919911833,
-0.458067593765231));
#37052=CARTESIAN_POINT('Ctrl Pts',(1.22124532708767E-15,2.28584270747282,
-0.439545337752037));
#37053=CARTESIAN_POINT('Ctrl Pts',(1.2524054674238E-15,2.29363652551706,
-0.356747287048907));
#37054=CARTESIAN_POINT('Ctrl Pts',(2.98674777348732E-15,2.29720513916532,
-0.273778886552983));
#37055=CARTESIAN_POINT('Ctrl Pts',(2.33146835171283E-15,2.29652846067949,
-0.19100810983232));
#37056=CARTESIAN_POINT('Ctrl Pts',(1.68915238065727E-15,2.29586516898396,
-0.109874794703355));
#37057=CARTESIAN_POINT('Ctrl Pts',(3.98927178069262E-15,2.29112266840023,
-0.0289304327025789));
#37058=CARTESIAN_POINT('Ctrl Pts',(4.63518112781003E-15,2.28223399867317,
0.0514685248767753));
#37059=CARTESIAN_POINT('Ctrl Pts',(5.26622813180739E-15,2.27354985681052,
0.130017506295588));
#37060=CARTESIAN_POINT('Ctrl Pts',(-5.74427027136191E-16,2.26090793882628,
0.208046647240463));
#37061=CARTESIAN_POINT('Ctrl Pts',(-3.33066907387547E-16,2.24420274952171,
0.285201797779823));
#37062=CARTESIAN_POINT('Ctrl Pts',(-2.43223168602901E-16,2.23798442038849,
0.313921982366105));
#37063=CARTESIAN_POINT('Ctrl Pts',(1.74108706017718E-15,2.2312026560155,
0.342520788687836));
#37064=CARTESIAN_POINT('Ctrl Pts',(1.74860126378462E-15,2.22385052915109,
0.370978839784131));
#37065=CARTESIAN_POINT('Ctrl Pts',(1.75230874467845E-15,2.22022301633633,
0.385019939310695));
#37066=CARTESIAN_POINT('Ctrl Pts',(-1.10164963276453E-15,2.21645664217309,
0.399026762935435));
#37067=CARTESIAN_POINT('Ctrl Pts',(-1.08246744900953E-15,2.21255050287209,
0.412996918792799));
#37068=CARTESIAN_POINT('Ctrl Pts',(-1.06630207080745E-15,2.20925868688716,
0.424769971113676));
#37069=CARTESIAN_POINT('Ctrl Pts',(3.14036835259962E-15,2.20587022064258,
0.436507639975992));
#37070=CARTESIAN_POINT('Ctrl Pts',(3.08086889333481E-15,2.20238504581408,
0.448208492551131));
#37071=CARTESIAN_POINT('Ctrl Pts',(2.70032584026761E-15,2.18009477484193,
0.523044099755827));
#37072=CARTESIAN_POINT('Ctrl Pts',(1.67653588062007E-15,2.15385146753471,
0.596378577822135));
#37073=CARTESIAN_POINT('Ctrl Pts',(1.72084568816899E-15,2.12359651477114,
0.667885141097565));
#37074=CARTESIAN_POINT('Ctrl Pts',(1.73741029882426E-15,2.11228611780386,
0.694616883921002));
#37075=CARTESIAN_POINT('Ctrl Pts',(-1.7751156820648E-15,2.10041461978735,
0.721092938851344));
#37076=CARTESIAN_POINT('Ctrl Pts',(-1.66533453693773E-15,2.08797732702981,
0.747295272013091));
#37077=CARTESIAN_POINT('Ctrl Pts',(-1.36557198820265E-15,2.05401671774622,
0.818841967598024));
#37078=CARTESIAN_POINT('Ctrl Pts',(2.10526653845581E-15,2.01584013144301,
0.888350571890128));
#37079=CARTESIAN_POINT('Ctrl Pts',(2.37310171513627E-15,1.97374114073884,
0.955596271977286));
#37080=CARTESIAN_POINT('Ctrl Pts',(2.63446996854363E-15,1.9326586369134,
1.02121831385681));
#37081=CARTESIAN_POINT('Ctrl Pts',(5.41294650752726E-16,1.88783990086501,
1.08468576120073));
#37082=CARTESIAN_POINT('Ctrl Pts',(5.68989300120393E-16,1.83953150843297,
1.14575058726299));
#37083=CARTESIAN_POINT('Ctrl Pts',(5.7480995700391E-16,1.82937840726139,
1.15858474145074));
#37084=CARTESIAN_POINT('Ctrl Pts',(2.09061406733528E-15,1.81906844436066,
1.17131562858466));
#37085=CARTESIAN_POINT('Ctrl Pts',(2.13717932240343E-15,1.80862151941036,
1.18391988280963));
#37086=CARTESIAN_POINT('Ctrl Pts',(2.358433526946E-15,1.75898309122153,
1.24380883302188));
#37087=CARTESIAN_POINT('Ctrl Pts',(3.18887734197556E-15,1.70618592804151,
1.30093322236681));
#37088=CARTESIAN_POINT('Ctrl Pts',(1.85962356624714E-15,1.65052993023653,
1.35510174998724));
#37089=CARTESIAN_POINT('Ctrl Pts',(5.3128362391325E-16,1.59491219473355,
1.40923303790945));
#37090=CARTESIAN_POINT('Ctrl Pts',(-1.69124579543603E-15,1.53643861743996,
1.46041303633541));
#37091=CARTESIAN_POINT('Ctrl Pts',(-2.27595720048157E-15,1.47538001259375,
1.50840761508891));
#37092=CARTESIAN_POINT('Ctrl Pts',(-2.85094123198906E-15,1.41533719066528,
1.55560374662331));
#37093=CARTESIAN_POINT('Ctrl Pts',(-1.60428500839505E-16,1.35279374628381,
1.59971990299823));
#37094=CARTESIAN_POINT('Ctrl Pts',(-8.11850586757146E-16,1.28799325731152,
1.64048554490097));
#37095=CARTESIAN_POINT('Ctrl Pts',(-1.06202854919824E-15,1.26310669812549,
1.65614154651545));
#37096=CARTESIAN_POINT('Ctrl Pts',(-6.10864375227674E-16,1.2378871606073,
1.671302834036));
#37097=CARTESIAN_POINT('Ctrl Pts',(-7.56339435525888E-16,1.21234829708237,
1.68595199882551));
#37098=CARTESIAN_POINT('Ctrl Pts',(-8.17640432114187E-16,1.20158660512911,
1.69212493595262));
#37099=CARTESIAN_POINT('Ctrl Pts',(1.56771109887162E-15,1.19076801370443,
1.69820693920532));
#37100=CARTESIAN_POINT('Ctrl Pts',(1.56125112837913E-15,1.17990651797273,
1.70418977564566));
#37101=CARTESIAN_POINT('Ctrl Pts',(1.52217870306378E-15,1.11421194842586,
1.74037630780726));
#37102=CARTESIAN_POINT('Ctrl Pts',(-3.32055172913184E-16,1.04683370283974,
1.77300608886991));
#37103=CARTESIAN_POINT('Ctrl Pts',(-4.85722573273506E-17,0.97802182017074,
1.80187351209679));
#37104=CARTESIAN_POINT('Ctrl Pts',(2.3032739167331E-16,0.910322467340964,
1.83027421550035));
#37105=CARTESIAN_POINT('Ctrl Pts',(-3.29174076884851E-16,0.841234638235302,
1.85503349815338));
#37106=CARTESIAN_POINT('Ctrl Pts',(-1.21430643318376E-16,0.770987551814153,
1.87590662840547));
#37107=CARTESIAN_POINT('Ctrl Pts',(7.96662066757932E-17,0.702987964255391,
1.8961119396933));
#37108=CARTESIAN_POINT('Ctrl Pts',(1.21052487671592E-16,0.633901450878722,
1.91267585920164));
#37109=CARTESIAN_POINT('Ctrl Pts',(-1.55257751099924E-16,0.563938259187892,
1.92532798546484));
#37110=CARTESIAN_POINT('Ctrl Pts',(-2.92932647256323E-16,0.529078258365518,
1.93163205938258));
#37111=CARTESIAN_POINT('Ctrl Pts',(6.23284630163641E-17,0.494000706321858,
1.93696420018631));
#37112=CARTESIAN_POINT('Ctrl Pts',(0.,0.458732584425967,1.94128616604711));
#37113=CARTESIAN_POINT('Ctrl Pts',(-0.307327496212056,-2.44646461313235,
-7.12799915801969E-5));
#37114=CARTESIAN_POINT('Ctrl Pts',(-0.286149307168018,-2.44640487853515,
-0.409278547049527));
#37115=CARTESIAN_POINT('Ctrl Pts',(-0.264971118123981,-2.34924893135542,
-0.818477401716759));
#37116=CARTESIAN_POINT('Ctrl Pts',(-0.243792929079942,-2.15510860587612,
-1.17470409077093));
#37117=CARTESIAN_POINT('Ctrl Pts',(-0.201549569558017,-1.76786399540107,
-1.88525644563605));
#37118=CARTESIAN_POINT('Ctrl Pts',(-0.15930621003609,-0.994749359521043,
-2.38504938492044));
#37119=CARTESIAN_POINT('Ctrl Pts',(-0.117062850514165,-0.187633739351079,
-2.4470817858882));
#37120=CARTESIAN_POINT('Ctrl Pts',(-0.0780419003427761,0.557913460342055,
-2.50438222919026));
#37121=CARTESIAN_POINT('Ctrl Pts',(-0.0390209501713872,1.33247216588429,
-2.18816135588657));
#37122=CARTESIAN_POINT('Ctrl Pts',(1.2490009027033E-15,1.8331192860662,
-1.63215490580856));
#37123=CARTESIAN_POINT('',(-11.6495,-1.16034898466906,-1.62253437445174));
#37124=CARTESIAN_POINT('Ctrl Pts',(-11.6495,-1.16282838272805,-1.62470001792843));
#37125=CARTESIAN_POINT('Ctrl Pts',(-11.6495,-1.20737062417396,-1.60007728866689));
#37126=CARTESIAN_POINT('Ctrl Pts',(-11.6495,-1.25082068484827,-1.57369074934353));
#37127=CARTESIAN_POINT('Ctrl Pts',(-11.6495,-1.2930601147943,-1.54556381430646));
#37128=CARTESIAN_POINT('Ctrl Pts',(-11.6495,-1.35275072455609,-1.50581626313832));
#37129=CARTESIAN_POINT('Ctrl Pts',(-11.6495,-1.4100250943243,-1.4625955098447));
#37130=CARTESIAN_POINT('Ctrl Pts',(-11.6495,-1.46480184196881,-1.41624486913394));
#37131=CARTESIAN_POINT('Ctrl Pts',(-11.6495,-1.49642999741264,-1.3894819572715));
#37132=CARTESIAN_POINT('Ctrl Pts',(-11.6495,-1.52722514655207,-1.36167461307911));
#37133=CARTESIAN_POINT('Ctrl Pts',(-11.6495,-1.55716837922547,-1.3328819584687));
#37134=CARTESIAN_POINT('Ctrl Pts',(-11.6495,-1.56777135753634,-1.3226864029094));
#37135=CARTESIAN_POINT('Ctrl Pts',(-11.6495,-1.57826909663807,-1.31236563771069));
#37136=CARTESIAN_POINT('Ctrl Pts',(-11.6495,-1.58865543938623,-1.30192742989216));
#37137=CARTESIAN_POINT('Ctrl Pts',(-11.6495,-1.64145689071544,-1.24886231010381));
#37138=CARTESIAN_POINT('Ctrl Pts',(-11.6495,-1.69128391428968,-1.19286573360743));
#37139=CARTESIAN_POINT('Ctrl Pts',(-11.6495,-1.73804986103682,-1.13431476634906));
#37140=CARTESIAN_POINT('Ctrl Pts',(-11.6495,-1.77743172266821,-1.08500867396049));
#37141=CARTESIAN_POINT('Ctrl Pts',(-11.6495,-1.81464268770884,-1.0338899671485));
#37142=CARTESIAN_POINT('Ctrl Pts',(-11.6495,-1.84961682596229,-0.981158846144615));
#37143=CARTESIAN_POINT('Ctrl Pts',(-11.6495,-1.86647192782428,-0.95574611375999));
#37144=CARTESIAN_POINT('Ctrl Pts',(-11.6495,-1.88280729537051,-0.929958580884817));
#37145=CARTESIAN_POINT('Ctrl Pts',(-11.6495,-1.89861422754426,-0.903817116040125));
#37146=CARTESIAN_POINT('Ctrl Pts',(-11.6495,-1.9058390612283,-0.891868704186114));
#37147=CARTESIAN_POINT('Ctrl Pts',(-11.6495,-1.91295470835595,-0.879844221187209));
#37148=CARTESIAN_POINT('Ctrl Pts',(-11.6495,-1.91995627982203,-0.86775251788438));
#37149=CARTESIAN_POINT('Ctrl Pts',(-11.6495,-1.95884003755814,-0.800600327248006));
#37150=CARTESIAN_POINT('Ctrl Pts',(-11.6495,-1.9941235221355,-0.731526978428571));
#37151=CARTESIAN_POINT('Ctrl Pts',(-11.6495,-2.02571637553995,-0.660913112382761));
#37152=CARTESIAN_POINT('Ctrl Pts',(-11.6495,-2.0584793484816,-0.587683886996029));
#37153=CARTESIAN_POINT('Ctrl Pts',(-11.6495,-2.08727405704258,-0.512797249958379));
#37154=CARTESIAN_POINT('Ctrl Pts',(-11.6495,-2.11196354206791,-0.436633606374266));
#37155=CARTESIAN_POINT('Ctrl Pts',(-11.6495,-2.13048065583691,-0.379510873686182));
#37156=CARTESIAN_POINT('Ctrl Pts',(-11.6495,-2.14668789055987,-0.32166880515796));
#37157=CARTESIAN_POINT('Ctrl Pts',(-11.6495,-2.1605106338825,-0.263256315368801));
#37158=CARTESIAN_POINT('Ctrl Pts',(-11.6495,-2.17087769137447,-0.219446948026931));
#37159=CARTESIAN_POINT('Ctrl Pts',(-11.6495,-2.17990318743524,-0.175316499307717));
#37160=CARTESIAN_POINT('Ctrl Pts',(-11.6495,-2.18754943061712,-0.130925494906403));
#37161=CARTESIAN_POINT('Ctrl Pts',(-11.6495,-2.18995384688195,-0.116966423705573));
#37162=CARTESIAN_POINT('Ctrl Pts',(-11.6495,-2.19222183574009,-0.102981577419542));
#37163=CARTESIAN_POINT('Ctrl Pts',(-11.6495,-2.19435210579768,-0.0889728138154531));
#37164=CARTESIAN_POINT('Ctrl Pts',(-11.6495,-2.19617602412986,-0.0769786346466959));
#37165=CARTESIAN_POINT('Ctrl Pts',(-11.6495,-2.19789753243822,-0.0649764515061904));
#37166=CARTESIAN_POINT('Ctrl Pts',(-11.6495,-2.19951620912844,-0.052968022700671));
#37167=CARTESIAN_POINT('Ctrl Pts',(-11.6495,-2.21033880808821,0.0273212715633298));
#37168=CARTESIAN_POINT('Ctrl Pts',(-11.6495,-2.21656893840084,0.10789384853219));
#37169=CARTESIAN_POINT('Ctrl Pts',(-11.6495,-2.21807674608418,0.188374054145962));
#37170=CARTESIAN_POINT('Ctrl Pts',(-11.6495,-2.21859286329889,0.215922142685333));
#37171=CARTESIAN_POINT('Ctrl Pts',(-11.6495,-2.21855530302174,0.243459652058912));
#37172=CARTESIAN_POINT('Ctrl Pts',(-11.6495,-2.21795761289143,0.270972168827435));
#37173=CARTESIAN_POINT('Ctrl Pts',(-11.6495,-2.21627102067576,0.348608379068655));
#37174=CARTESIAN_POINT('Ctrl Pts',(-11.6495,-2.2101281442622,0.426045052693772));
#37175=CARTESIAN_POINT('Ctrl Pts',(-11.6495,-2.1997617102457,0.503031799881565));
#37176=CARTESIAN_POINT('Ctrl Pts',(-11.6495,-2.18918095360188,0.58161022284716));
#37177=CARTESIAN_POINT('Ctrl Pts',(-11.6495,-2.17420007249142,0.659720697636032));
#37178=CARTESIAN_POINT('Ctrl Pts',(-11.6495,-2.15501262324688,0.737098841831874));
#37179=CARTESIAN_POINT('Ctrl Pts',(-11.6495,-2.15035875822838,0.755866705860072));
#37180=CARTESIAN_POINT('Ctrl Pts',(-11.6495,-2.14545522714254,0.774598052202702));
#37181=CARTESIAN_POINT('Ctrl Pts',(-11.6495,-2.14031447676813,0.793253811565047));
#37182=CARTESIAN_POINT('Ctrl Pts',(-11.6495,-2.11881533699752,0.871274090482765));
#37183=CARTESIAN_POINT('Ctrl Pts',(-11.6495,-2.09315279746427,0.948060275340426));
#37184=CARTESIAN_POINT('Ctrl Pts',(-11.6495,-2.06360314980312,1.02334283907926));
#37185=CARTESIAN_POINT('Ctrl Pts',(-11.6495,-2.03346473222344,1.10012539054816));
#37186=CARTESIAN_POINT('Ctrl Pts',(-11.6495,-1.99928257575015,1.17534462999745));
#37187=CARTESIAN_POINT('Ctrl Pts',(-11.6495,-1.9612944536973,1.24871635014604));
#37188=CARTESIAN_POINT('Ctrl Pts',(-11.6495,-1.92301128002754,1.3226579443367));
#37189=CARTESIAN_POINT('Ctrl Pts',(-11.6495,-1.88086246501352,1.39472412259045));
#37190=CARTESIAN_POINT('Ctrl Pts',(-11.6495,-1.83503975229434,1.46461255055414));
#37191=CARTESIAN_POINT('Ctrl Pts',(-11.6495,-1.81559616867206,1.49426774582094));
#37192=CARTESIAN_POINT('Ctrl Pts',(-11.6495,-1.79549050001335,1.52353061819257));
#37193=CARTESIAN_POINT('Ctrl Pts',(-11.6495,-1.77473484362459,1.5523768230785));
#37194=CARTESIAN_POINT('Ctrl Pts',(-11.6495,-1.76427959115328,1.56690752975781));
#37195=CARTESIAN_POINT('Ctrl Pts',(-11.6495,-1.75365636602808,1.58133631474072));
#37196=CARTESIAN_POINT('Ctrl Pts',(-11.6495,-1.74288499727145,1.59563608488518));
#37197=CARTESIAN_POINT('Ctrl Pts',(-11.6495,-1.69122789171288,1.66421462420599));
#37198=CARTESIAN_POINT('Ctrl Pts',(-11.6495,-1.63610074686772,1.72992393044111));
#37199=CARTESIAN_POINT('Ctrl Pts',(-11.6495,-1.5777607315452,1.79246828497059));
#37200=CARTESIAN_POINT('Ctrl Pts',(-11.6495,-1.51932500291965,1.85511525049058));
#37201=CARTESIAN_POINT('Ctrl Pts',(-11.6495,-1.45766541888288,1.91458780561411));
#37202=CARTESIAN_POINT('Ctrl Pts',(-11.6495,-1.39299120107362,1.97057137326597));
#37203=CARTESIAN_POINT('Ctrl Pts',(-11.6495,-1.32967814016095,2.02537669057656));
#37204=CARTESIAN_POINT('Ctrl Pts',(-11.6495,-1.26347544514419,2.07683912052618));
#37205=CARTESIAN_POINT('Ctrl Pts',(-11.6495,-1.19453988778704,2.12463431235531));
#37206=CARTESIAN_POINT('Ctrl Pts',(-11.6495,-1.15558812056379,2.15164079867228));
#37207=CARTESIAN_POINT('Ctrl Pts',(-11.6495,-1.11576313904794,2.17747582457847));
#37208=CARTESIAN_POINT('Ctrl Pts',(-11.6495,-1.07508846035129,2.20207516956608));
#37209=CARTESIAN_POINT('Ctrl Pts',(-11.6495,-1.16282838272804,-1.62470001792844));
#37210=CARTESIAN_POINT('Ctrl Pts',(-11.6104790498286,-0.66559499343731,
-1.97639595858999));
#37211=CARTESIAN_POINT('Ctrl Pts',(-11.5292147401353,0.733321543403064,
-2.21002070237282));
#37212=CARTESIAN_POINT('Ctrl Pts',(-11.4057070709201,2.2660422239822,-0.644398977329155));
#37213=CARTESIAN_POINT('Ctrl Pts',(-11.2789769923543,1.77364945549679,1.55095382729707));
#37214=CARTESIAN_POINT('Ctrl Pts',(-11.1522469137885,-0.335801440579385,
2.33175063016555));
#37215=CARTESIAN_POINT('Ctrl Pts',(-11.0494062101355,-1.79909114547032,
1.24084066535289));
#37216=CARTESIAN_POINT('Ctrl Pts',(-10.9888088660044,-1.99263284951445,
0.289271291292402));
#37217=CARTESIAN_POINT('Ctrl Pts',(-10.9704548813952,-1.99173416440345,
0.000704422997178135));
#37218=CARTESIAN_POINT('Origin',(-11.6495,-5.69858952725515E-16,8.58067791224701E-17));
#37219=CARTESIAN_POINT('',(-11.6495,-2.4505,-3.00099698131059E-16));
#37220=CARTESIAN_POINT('Origin',(-11.6495,0.,0.));
#37221=CARTESIAN_POINT('Origin',(-11.6495,0.,0.));
#37222=CARTESIAN_POINT('',(-11.6495,1.16034898466908,-1.62253437445172));
#37223=CARTESIAN_POINT('Ctrl Pts',(-11.6495,1.07765118568552,2.20520362934387));
#37224=CARTESIAN_POINT('Ctrl Pts',(-11.6495,1.13073687254156,2.17343691132479));
#37225=CARTESIAN_POINT('Ctrl Pts',(-11.6495,1.18244979581025,2.13957757514889));
#37226=CARTESIAN_POINT('Ctrl Pts',(-11.6495,1.23264818481424,2.10361864746718));
#37227=CARTESIAN_POINT('Ctrl Pts',(-11.6495,1.30197054661187,2.05396052408779));
#37228=CARTESIAN_POINT('Ctrl Pts',(-11.6495,1.36840639937506,2.00029914630137));
#37229=CARTESIAN_POINT('Ctrl Pts',(-11.6495,1.43178638700421,1.9429963843878));
#37230=CARTESIAN_POINT('Ctrl Pts',(-11.6495,1.46369654011807,1.9141459542298));
#37231=CARTESIAN_POINT('Ctrl Pts',(-11.6495,1.49483142030138,1.88437196977866));
#37232=CARTESIAN_POINT('Ctrl Pts',(-11.6495,1.52516517286246,1.85371813290651));
#37233=CARTESIAN_POINT('Ctrl Pts',(-11.6495,1.5399621404638,1.83876502645716));
#37234=CARTESIAN_POINT('Ctrl Pts',(-11.6495,1.55456843151077,1.82360253561288));
#37235=CARTESIAN_POINT('Ctrl Pts',(-11.6495,1.56898078085552,1.80823563715035));
#37236=CARTESIAN_POINT('Ctrl Pts',(-11.6495,1.58070094654556,1.79573922925633));
#37237=CARTESIAN_POINT('Ctrl Pts',(-11.6495,1.59228652143182,1.78311435458078));
#37238=CARTESIAN_POINT('Ctrl Pts',(-11.6495,1.60373329040506,1.77036734183654));
#37239=CARTESIAN_POINT('Ctrl Pts',(-11.6495,1.66048032516668,1.70717438520439));
#37240=CARTESIAN_POINT('Ctrl Pts',(-11.6495,1.71384375789451,1.64095615253125));
#37241=CARTESIAN_POINT('Ctrl Pts',(-11.6495,1.76365444232725,1.57207081711976));
#37242=CARTESIAN_POINT('Ctrl Pts',(-11.6495,1.80211943702331,1.51887592346563));
#37243=CARTESIAN_POINT('Ctrl Pts',(-11.6495,1.83846500194502,1.46408976223796));
#37244=CARTESIAN_POINT('Ctrl Pts',(-11.6495,1.87259337417673,1.40786969807678));
#37245=CARTESIAN_POINT('Ctrl Pts',(-11.6495,1.88968256071726,1.3797184825061));
#37246=CARTESIAN_POINT('Ctrl Pts',(-11.6495,1.90621554079354,1.35120766875282));
#37247=CARTESIAN_POINT('Ctrl Pts',(-11.6495,1.9221782719748,1.32235676032253));
#37248=CARTESIAN_POINT('Ctrl Pts',(-11.6495,1.93118753982307,1.3060734840609));
#37249=CARTESIAN_POINT('Ctrl Pts',(-11.6495,1.9400170008051,1.28967806812594));
#37250=CARTESIAN_POINT('Ctrl Pts',(-11.6495,1.94865127865783,1.27319896184839));
#37251=CARTESIAN_POINT('Ctrl Pts',(-11.6495,1.98724824363966,1.19953403019175));
#37252=CARTESIAN_POINT('Ctrl Pts',(-11.6495,2.02199988085258,1.12410988628387));
#37253=CARTESIAN_POINT('Ctrl Pts',(-11.6495,2.05274812180369,1.04725942698306));
#37254=CARTESIAN_POINT('Ctrl Pts',(-11.6495,2.08288806559826,0.971929312080035));
#37255=CARTESIAN_POINT('Ctrl Pts',(-11.6495,2.10918158952032,0.895227812752492));
#37256=CARTESIAN_POINT('Ctrl Pts',(-11.6495,2.13143161793832,0.817459396317668));
#37257=CARTESIAN_POINT('Ctrl Pts',(-11.6495,2.15316968868661,0.741480377024631));
#37258=CARTESIAN_POINT('Ctrl Pts',(-11.6495,2.17104828296331,0.66448219410781));
#37259=CARTESIAN_POINT('Ctrl Pts',(-11.6495,2.18483553769043,0.58675257912323));
#37260=CARTESIAN_POINT('Ctrl Pts',(-11.6495,2.18996770971013,0.557818482885722));
#37261=CARTESIAN_POINT('Ctrl Pts',(-11.6495,2.19453248101047,0.528783133929868));
#37262=CARTESIAN_POINT('Ctrl Pts',(-11.6495,2.19851609634267,0.499661837442922));
#37263=CARTESIAN_POINT('Ctrl Pts',(-11.6495,2.20048159642361,0.485293504702629));
#37264=CARTESIAN_POINT('Ctrl Pts',(-11.6495,2.20230560473944,0.470904253929722));
#37265=CARTESIAN_POINT('Ctrl Pts',(-11.6495,2.20398637829912,0.456495955912551));
#37266=CARTESIAN_POINT('Ctrl Pts',(-11.6495,2.20540279415176,0.444353843369362));
#37267=CARTESIAN_POINT('Ctrl Pts',(-11.6495,2.20671636256573,0.43220783876865));
#37268=CARTESIAN_POINT('Ctrl Pts',(-11.6495,2.2079264865813,0.420059244968361));
#37269=CARTESIAN_POINT('Ctrl Pts',(-11.6495,2.21566622029946,0.342359042464759));
#37270=CARTESIAN_POINT('Ctrl Pts',(-11.6495,2.21917890730586,0.264549530424612));
#37271=CARTESIAN_POINT('Ctrl Pts',(-11.6495,2.21828644435235,0.186910890393313));
#37272=CARTESIAN_POINT('Ctrl Pts',(-11.6495,2.21795281039612,0.157886843481426));
#37273=CARTESIAN_POINT('Ctrl Pts',(-11.6495,2.21700303246508,0.128886715398128));
#37274=CARTESIAN_POINT('Ctrl Pts',(-11.6495,2.21542593150821,0.0999254148515203));
#37275=CARTESIAN_POINT('Ctrl Pts',(-11.6495,2.21111957118993,0.0208450015803043));
#37276=CARTESIAN_POINT('Ctrl Pts',(-11.6495,2.20213931188017,-0.0579475015914385));
#37277=CARTESIAN_POINT('Ctrl Pts',(-11.6495,2.18867160105417,-0.136132775928427));
#37278=CARTESIAN_POINT('Ctrl Pts',(-11.6495,2.1755290745819,-0.212430229221862));
#37279=CARTESIAN_POINT('Ctrl Pts',(-11.6495,2.15811243339091,-0.288150111668693));
#37280=CARTESIAN_POINT('Ctrl Pts',(-11.6495,2.13655583598888,-0.362969437792645));
#37281=CARTESIAN_POINT('Ctrl Pts',(-11.6495,2.13202523535206,-0.378694391052281));
#37282=CARTESIAN_POINT('Ctrl Pts',(-11.6495,2.12731033581924,-0.394383242756282));
#37283=CARTESIAN_POINT('Ctrl Pts',(-11.6495,2.1224206951262,-0.410006827745426));
#37284=CARTESIAN_POINT('Ctrl Pts',(-11.6495,2.09918759635712,-0.484242199210638));
#37285=CARTESIAN_POINT('Ctrl Pts',(-11.6495,2.07198357162087,-0.557116646646277));
#37286=CARTESIAN_POINT('Ctrl Pts',(-11.6495,2.04101362673087,-0.628339464180321));
#37287=CARTESIAN_POINT('Ctrl Pts',(-11.6495,2.01006498584023,-0.699513288057304));
#37288=CARTESIAN_POINT('Ctrl Pts',(-11.6495,1.97535493052193,-0.769038579984836));
#37289=CARTESIAN_POINT('Ctrl Pts',(-11.6495,1.93704531624577,-0.83659602647624));
#37290=CARTESIAN_POINT('Ctrl Pts',(-11.6495,1.89937304271498,-0.903029548487702));
#37291=CARTESIAN_POINT('Ctrl Pts',(-11.6495,1.85821928820994,-0.967560808242973));
#37292=CARTESIAN_POINT('Ctrl Pts',(-11.6495,1.81370690330138,-1.02984712465529));
#37293=CARTESIAN_POINT('Ctrl Pts',(-11.6495,1.79661192966788,-1.05376817357198));
#37294=CARTESIAN_POINT('Ctrl Pts',(-11.6495,1.7790213017759,-1.07735764126509));
#37295=CARTESIAN_POINT('Ctrl Pts',(-11.6495,1.76094105430332,-1.10059424300847));
#37296=CARTESIAN_POINT('Ctrl Pts',(-11.6495,1.753322321499,-1.11038578265591));
#37297=CARTESIAN_POINT('Ctrl Pts',(-11.6495,1.74561646654128,-1.12011474214072));
#37298=CARTESIAN_POINT('Ctrl Pts',(-11.6495,1.73783331949158,-1.12976819796877));
#37299=CARTESIAN_POINT('Ctrl Pts',(-11.6495,1.69075783958123,-1.18815602785256));
#37300=CARTESIAN_POINT('Ctrl Pts',(-11.6495,1.64077613345497,-1.2438907292167));
#37301=CARTESIAN_POINT('Ctrl Pts',(-11.6495,1.58804164355534,-1.29668725875532));
#37302=CARTESIAN_POINT('Ctrl Pts',(-11.6495,1.53615976281906,-1.34863017607615));
#37303=CARTESIAN_POINT('Ctrl Pts',(-11.6495,1.48161273193739,-1.39772971703901));
#37304=CARTESIAN_POINT('Ctrl Pts',(-11.6495,1.42451989663264,-1.44367252532997));
#37305=CARTESIAN_POINT('Ctrl Pts',(-11.6495,1.36925371315748,-1.48814542037571));
#37306=CARTESIAN_POINT('Ctrl Pts',(-11.6495,1.31160143729427,-1.52966066226345));
#37307=CARTESIAN_POINT('Ctrl Pts',(-11.6495,1.25165512889375,-1.56788833203711));
#37308=CARTESIAN_POINT('Ctrl Pts',(-11.6495,1.2217859935916,-1.58693583423069));
#37309=CARTESIAN_POINT('Ctrl Pts',(-11.6495,1.19134712145188,-1.60516638714514));
#37310=CARTESIAN_POINT('Ctrl Pts',(-11.6495,1.16034898466911,-1.6225343744517));
#37311=CARTESIAN_POINT('Origin',(-11.6495,0.,0.));
#37312=CARTESIAN_POINT('Origin',(-13.1285451186048,0.,0.));
#37313=CARTESIAN_POINT('Ctrl Pts',(-11.6495,1.16034898466908,-1.62253437445172));
#37314=CARTESIAN_POINT('Ctrl Pts',(-11.6072566404781,1.69867111894511,-1.23755544779991));
#37315=CARTESIAN_POINT('Ctrl Pts',(-11.5227699214342,2.35295738103105,0.103500486870383));
#37316=CARTESIAN_POINT('Ctrl Pts',(-11.3960398428684,1.19148277972948,2.03419922420614));
#37317=CARTESIAN_POINT('Ctrl Pts',(-11.2693097643027,-1.05708502050599,
2.10468425318621));
#37318=CARTESIAN_POINT('Ctrl Pts',(-11.1801448562148,-1.96080296173452,
0.806515742280787));
#37319=CARTESIAN_POINT('Ctrl Pts',(-11.1332233076488,-1.99752919412992,
0.0744005420673237));
#37320=CARTESIAN_POINT('Ctrl Pts',(-11.1285451186048,-1.99700380788516,
0.00135048458759495));
#37321=CARTESIAN_POINT('Ctrl Pts',(-11.9126273851832,1.42545942445495,-1.99324250386965));
#37322=CARTESIAN_POINT('Ctrl Pts',(-11.8703840256612,2.08677457173828,-1.52030561465535));
#37323=CARTESIAN_POINT('Ctrl Pts',(-11.7858973066174,2.89054872150224,0.12714773434053));
#37324=CARTESIAN_POINT('Ctrl Pts',(-11.6591672280516,1.46370650544038,2.49896237569475));
#37325=CARTESIAN_POINT('Ctrl Pts',(-11.5324371494858,-1.29860225228717,
2.58555145378261));
#37326=CARTESIAN_POINT('Ctrl Pts',(-11.4057070709201,-2.87652186863451,
0.318908881767984));
#37327=CARTESIAN_POINT('Ctrl Pts',(-11.2789769923543,-1.83266175101893,
-2.24033061384541));
#37328=CARTESIAN_POINT('Ctrl Pts',(-11.1522469137885,0.881950637603053,
-2.75638944163318));
#37329=CARTESIAN_POINT('Ctrl Pts',(-11.0255168352227,2.79252215107582,-0.760360236683921));
#37330=CARTESIAN_POINT('Ctrl Pts',(-10.898786756657,2.15759767705332,1.9290533008961));
#37331=CARTESIAN_POINT('Ctrl Pts',(-10.7720566780912,-0.4441263759771,2.85988114430123));
#37332=CARTESIAN_POINT('Ctrl Pts',(-10.6453265995254,-2.64099042545161,
1.18383794202982));
#37333=CARTESIAN_POINT('Ctrl Pts',(-10.5185965209596,-2.43044697619487,
-1.57138082209723));
#37334=CARTESIAN_POINT('Ctrl Pts',(-10.3918664423938,-0.00440784228849815,
-2.89417510655402));
#37335=CARTESIAN_POINT('Ctrl Pts',(-10.2651363638281,2.42564737449796,-1.57877333949545));
#37336=CARTESIAN_POINT('Ctrl Pts',(-10.1384062852623,2.64458668371764,1.17577667845936));
#37337=CARTESIAN_POINT('Ctrl Pts',(-10.0116762066965,0.452832795037591,
2.85853574486283));
#37338=CARTESIAN_POINT('Ctrl Pts',(-9.88494612813071,-2.15170392079859,
1.93557684058089));
#37339=CARTESIAN_POINT('Ctrl Pts',(-9.75821604956493,-2.79483906169062,
-0.75177235279057));
#37340=CARTESIAN_POINT('Ctrl Pts',(-9.63148597099916,-0.890317783065174,
-2.75383743537073));
#37341=CARTESIAN_POINT('Ctrl Pts',(-9.50475589243338,1.82577925575169,-2.24562173688547));
#37342=CARTESIAN_POINT('Ctrl Pts',(-9.3780258138676,2.87757364909028,0.309607283664348));
#37343=CARTESIAN_POINT('Ctrl Pts',(-9.25129573530183,1.30629435926593,2.58261141914626));
#37344=CARTESIAN_POINT('Ctrl Pts',(-9.12456565673605,-1.45574726827538,
2.50141693041908));
#37345=CARTESIAN_POINT('Ctrl Pts',(-8.99783557817026,-2.89079164405769,
0.140037208434977));
#37346=CARTESIAN_POINT('Ctrl Pts',(-8.8711054996045,-1.69071338440342,-2.34899446401371));
#37347=CARTESIAN_POINT('Ctrl Pts',(-8.7443754210387,1.05054724076537,-2.69678275833015));
#37348=CARTESIAN_POINT('Ctrl Pts',(-8.61764534247293,2.8341737118076,-0.586298659768404));
#37349=CARTESIAN_POINT('Ctrl Pts',(-8.49091526390716,2.03428804621161,2.05863034353453));
#37350=CARTESIAN_POINT('Ctrl Pts',(-8.36418518534136,-0.619968025159372,
2.8269995393587));
#37351=CARTESIAN_POINT('Ctrl Pts',(-8.23745510677561,-2.709087630006,1.01839626869896));
#37352=CARTESIAN_POINT('Ctrl Pts',(-8.11072502820981,-2.32871824705604,
-1.71853369851118));
#37353=CARTESIAN_POINT('Ctrl Pts',(-7.98399494964404,0.174411582240062,
-2.88892148513446));
#37354=CARTESIAN_POINT('Ctrl Pts',(-7.85726487107826,2.51855523593771,-1.42589139513639));
#37355=CARTESIAN_POINT('Ctrl Pts',(-7.73053479251247,2.5668911234533,1.33692060629286));
#37356=CARTESIAN_POINT('Ctrl Pts',(-7.60380471394671,0.275358306856354,
2.88105268089038));
#37357=CARTESIAN_POINT('Ctrl Pts',(-7.47707463538091,-2.26717942332955,
1.79893974597155));
#37358=CARTESIAN_POINT('Ctrl Pts',(-7.35034455681516,-2.74305287983666,
-0.92301010050071));
#37359=CARTESIAN_POINT('Ctrl Pts',(-7.22361447824936,-0.718476072358019,
-2.80358322163957));
#37360=CARTESIAN_POINT('Ctrl Pts',(-7.0968843996836,1.96103294514159,-2.12852919530761));
#37361=CARTESIAN_POINT('Ctrl Pts',(-6.97015432111781,2.85294778922629,0.486801457636237));
#37362=CARTESIAN_POINT('Ctrl Pts',(-6.84342424255203,1.14423684693021,2.6583846195266));
#37363=CARTESIAN_POINT('Ctrl Pts',(-6.71669416398626,-1.60751170758271,
2.40669750014258));
#37364=CARTESIAN_POINT('Ctrl Pts',(-6.58996408542048,-2.89392100336966,
-0.0388326340083757));
#37365=CARTESIAN_POINT('Ctrl Pts',(-6.4632340068547,-1.54235507453701,-2.44896459167096));
#37366=CARTESIAN_POINT('Ctrl Pts',(-6.33650392828892,1.21515609933081,-2.62672465276953));
#37367=CARTESIAN_POINT('Ctrl Pts',(-6.20977384972314,2.86498268873778,-0.410074310876727));
#37368=CARTESIAN_POINT('Ctrl Pts',(-6.08304377115736,1.90321298956112,2.18038232050574));
#37369=CARTESIAN_POINT('Ctrl Pts',(-5.95631369259159,-0.793444672276071,
2.78329522315633));
#37370=CARTESIAN_POINT('Ctrl Pts',(-5.8295836140258,-2.7668319389872,0.849074654319879));
#37371=CARTESIAN_POINT('Ctrl Pts',(-5.70285353546003,-2.21809296340086,
-1.85912623372372));
#37372=CARTESIAN_POINT('Ctrl Pts',(-5.57612345689425,0.352565158057603,
-2.87262676944498));
#37373=CARTESIAN_POINT('Ctrl Pts',(-5.44939337832847,2.6018398862109,-1.26756299793353));
#37374=CARTESIAN_POINT('Ctrl Pts',(-5.3226632997627,2.47938810549972,1.49295725642586));
#37375=CARTESIAN_POINT('Ctrl Pts',(-5.19593322119691,0.0968316478091236,
2.89256121442409));
#37376=CARTESIAN_POINT('Ctrl Pts',(-5.06920314263115,-2.37399241897732,
1.65542947353446));
#37377=CARTESIAN_POINT('Ctrl Pts',(-4.94247306406535,-2.68078603109511,
-1.09072132219616));
#37378=CARTESIAN_POINT('Ctrl Pts',(-4.81574298549958,-0.543889188532094,
-2.84261698049623));
#37379=CARTESIAN_POINT('Ctrl Pts',(-4.6890129069338,2.08879389097954,-2.00330397798648));
#37380=CARTESIAN_POINT('Ctrl Pts',(-4.56228282836802,2.8174213562132,0.662135672472256));
#37381=CARTESIAN_POINT('Ctrl Pts',(-4.43555274980224,0.977807419436725,
2.7240006236599));
#37382=CARTESIAN_POINT('Ctrl Pts',(-4.30882267123646,-1.75313414650703,
2.30278253675232));
#37383=CARTESIAN_POINT('Ctrl Pts',(-4.18209259267069,-2.88599323592512,
-0.217554106806299));
#37384=CARTESIAN_POINT('Ctrl Pts',(-4.05536251410491,-1.38810371613861,
-2.53957768544997));
#37385=CARTESIAN_POINT('Ctrl Pts',(-3.92863243553913,1.37512207515111,-2.54663032765321));
#37386=CARTESIAN_POINT('Ctrl Pts',(-3.80190235697336,2.8848451063612,-0.232283144877331));
#37387=CARTESIAN_POINT('Ctrl Pts',(-3.67517227840757,1.76486611447052,2.29380346698343));
#37388=CARTESIAN_POINT('Ctrl Pts',(-3.5484421998418,-0.963889716762702,
2.72895646020112));
#37389=CARTESIAN_POINT('Ctrl Pts',(-3.42171212127602,-2.81400470402705,
0.676508885377088));
#37390=CARTESIAN_POINT('Ctrl Pts',(-3.29498204271024,-2.09899276446139,
-1.99261539738261));
#37391=CARTESIAN_POINT('Ctrl Pts',(-3.16825196414446,0.529371649267236,
-2.84535628835101));
#37392=CARTESIAN_POINT('Ctrl Pts',(-3.04152188557868,2.67518339532782,-1.10439148019637));
#37393=CARTESIAN_POINT('Ctrl Pts',(-2.91479180701291,2.38241181420258,1.64328959609923));
#37394=CARTESIAN_POINT('Ctrl Pts',(-2.78806172844712,-0.0820649900061464,
2.89301781990601));
#37395=CARTESIAN_POINT('Ctrl Pts',(-2.66133164988135,-2.47173483038822,
1.50559410984514));
#37396=CARTESIAN_POINT('Ctrl Pts',(-2.53460157131557,-2.60827641565575,
-1.25426508983179));
#37397=CARTESIAN_POINT('Ctrl Pts',(-2.40787149274979,-0.367224183821934,
-2.87078966048055));
#37398=CARTESIAN_POINT('Ctrl Pts',(-2.28114141418401,2.20857390538749,-1.87042446512356));
#37399=CARTESIAN_POINT('Ctrl Pts',(-2.15441133561824,2.77113016932584,0.83493989952818));
#37400=CARTESIAN_POINT('Ctrl Pts',(-2.02768125705246,0.807641816455084,
2.77920890990336));
#37401=CARTESIAN_POINT('Ctrl Pts',(-1.90095117848668,-1.89205788973094,
2.19006874020588));
#37402=CARTESIAN_POINT('Ctrl Pts',(-1.7742210999209,-2.86703920430662,-0.395443708098236));
#37403=CARTESIAN_POINT('Ctrl Pts',(-1.64749102135512,-1.22854758315733,
-2.62048874808283));
#37404=CARTESIAN_POINT('Ctrl Pts',(-1.52076094278934,1.52983188688595,-2.45680348712256));
#37405=CARTESIAN_POINT('Ctrl Pts',(-1.39403086422356,2.893689043194,-0.0536088933736343));
#37406=CARTESIAN_POINT('Ctrl Pts',(-1.26730078565778,1.61976845006142,2.39846885918956));
#37407=CARTESIAN_POINT('Ctrl Pts',(-1.140570707092,-1.13063748919579,2.66417478131471));
#37408=CARTESIAN_POINT('Ctrl Pts',(-1.01384062852623,-2.85045320367203,
0.501388978139588));
#37409=CARTESIAN_POINT('Ctrl Pts',(-0.887110549960449,-1.97182024087482,
-2.11854964337763));
#37410=CARTESIAN_POINT('Ctrl Pts',(-0.760380471394671,0.704055462274761,
-2.80710270335027));
#37411=CARTESIAN_POINT('Ctrl Pts',(-0.633650392828892,2.73849632864145,
-0.937213001936086));
#37412=CARTESIAN_POINT('Ctrl Pts',(-0.506920314263115,2.27596874940147,
1.7877491958748));
#37413=CARTESIAN_POINT('Ctrl Pts',(-0.380190235697335,-0.259952027690717,
2.88164346738145));
#37414=CARTESIAN_POINT('Ctrl Pts',(-0.253460157131559,-2.56137725938084,
1.35151626861576));
#37415=CARTESIAN_POINT('Ctrl Pts',(-0.126730078565777,-2.5230909281715,
-1.41613933844973));
#37416=CARTESIAN_POINT('Ctrl Pts',(-0.0422433595219261,-0.971443343070606,
-2.3921235558411));
#37417=CARTESIAN_POINT('Ctrl Pts',(0.,-0.160158266245241,-2.44526063636442));
#37418=CARTESIAN_POINT('Ctrl Pts',(-11.8249182567888,1.33708927785966,-1.86967312739701));
#37419=CARTESIAN_POINT('Ctrl Pts',(-11.7826748972669,1.95740675414056,-1.42605555903687));
#37420=CARTESIAN_POINT('Ctrl Pts',(-11.698188178223,2.71135160801184,0.119265318517148));
#37421=CARTESIAN_POINT('Ctrl Pts',(-11.5714580996572,1.37296526353675,2.34404132519854));
#37422=CARTESIAN_POINT('Ctrl Pts',(-11.4447280210914,-1.21809650836011,
2.42526238691714));
#37423=CARTESIAN_POINT('Ctrl Pts',(-11.3179979425257,-2.69819433797679,
0.299138396443103));
#37424=CARTESIAN_POINT('Ctrl Pts',(-11.1912678639599,-1.71904744196269,
-2.10144321980882));
#37425=CARTESIAN_POINT('Ctrl Pts',(-11.0645377853941,0.827274856730104,
-2.58550941877739));
#37426=CARTESIAN_POINT('Ctrl Pts',(-10.9378077068283,2.6194021115801,-0.713222349467867));
#37427=CARTESIAN_POINT('Ctrl Pts',(-10.8110776282626,2.02383924118076,1.80946327955578));
#37428=CARTESIAN_POINT('Ctrl Pts',(-10.6843475496968,-0.416593138426741,
2.68258524121815));
#37429=CARTESIAN_POINT('Ctrl Pts',(-10.557617471131,-2.47726446661335,1.11044691406543));
#37430=CARTESIAN_POINT('Ctrl Pts',(-10.4308873925652,-2.27977347971104,
-1.47396440236374));
#37431=CARTESIAN_POINT('Ctrl Pts',(-10.3041573139994,-0.00413458184871249,
-2.71475317840167));
#37432=CARTESIAN_POINT('Ctrl Pts',(-10.1774272354337,2.27527142524578,-1.48089862692316));
#37433=CARTESIAN_POINT('Ctrl Pts',(-10.0506971568679,2.4806377779019,1.10288540168486));
#37434=CARTESIAN_POINT('Ctrl Pts',(-9.9239670783021,0.424759810430573,2.68132324867549));
#37435=CARTESIAN_POINT('Ctrl Pts',(-9.79723699973633,-2.0183108633404,1.81558239793723));
#37436=CARTESIAN_POINT('Ctrl Pts',(-9.67050692117055,-2.62157538728873,
-0.705166864144143));
#37437=CARTESIAN_POINT('Ctrl Pts',(-9.54377684260478,-0.835123288114206,
-2.58311562197616));
#37438=CARTESIAN_POINT('Ctrl Pts',(-9.41704676403898,1.71259162114532,-2.10640632416894));
#37439=CARTESIAN_POINT('Ctrl Pts',(-9.29031668547322,2.69918091419632,0.290413443015511));
#37440=CARTESIAN_POINT('Ctrl Pts',(-9.16358660690742,1.22531174969842,2.42250461723157));
#37441=CARTESIAN_POINT('Ctrl Pts',(-9.03685652834166,-1.36549945252126,
2.346343711887));
#37442=CARTESIAN_POINT('Ctrl Pts',(-8.91012644977587,-2.71157947078975,
0.131355720610133));
#37443=CARTESIAN_POINT('Ctrl Pts',(-8.7833963712101,-1.58589904380056,-2.20337054685746));
#37444=CARTESIAN_POINT('Ctrl Pts',(-8.65666629264431,0.985419456642577,
-2.52959800119093));
#37445=CARTESIAN_POINT('Ctrl Pts',(-8.52993621407854,2.65847151917259,-0.549951572209463));
#37446=CARTESIAN_POINT('Ctrl Pts',(-8.40320613551276,1.90817408619515,1.93100730346573));
#37447=CARTESIAN_POINT('Ctrl Pts',(-8.276476056947,-0.581533633883264,2.65174210345273));
#37448=CARTESIAN_POINT('Ctrl Pts',(-8.14974597838119,-2.54114004279588,
0.955261656788515));
#37449=CARTESIAN_POINT('Ctrl Pts',(-8.02301589981544,-2.18435133675258,
-1.61199466115875));
#37450=CARTESIAN_POINT('Ctrl Pts',(-7.89628582124963,0.163599084300075,
-2.70982525078093));
#37451=CARTESIAN_POINT('Ctrl Pts',(-7.76955574268389,2.36241954270795,-1.33749446888549));
#37452=CARTESIAN_POINT('Ctrl Pts',(-7.64282566411808,2.40775888792125,1.25403934854711));
#37453=CARTESIAN_POINT('Ctrl Pts',(-7.51609558555232,0.258287702442303,
2.70244426637418));
#37454=CARTESIAN_POINT('Ctrl Pts',(-7.38936550698653,-2.12662756014756,
1.6874160039833));
#37455=CARTESIAN_POINT('Ctrl Pts',(-7.26263542842076,-2.57299964580475,
-0.86578887309092));
#37456=CARTESIAN_POINT('Ctrl Pts',(-7.13590534985498,-0.673934758343563,
-2.62977746046671));
#37457=CARTESIAN_POINT('Ctrl Pts',(-7.0091752712892,1.83946037291168,-1.99657283527748));
#37458=CARTESIAN_POINT('Ctrl Pts',(-6.88244519272341,2.67608171360365,0.456622614635815));
#37459=CARTESIAN_POINT('Ctrl Pts',(-6.75571511415765,1.07330085522939,2.49358032239687));
#37460=CARTESIAN_POINT('Ctrl Pts',(-6.62898503559186,-1.50785538428396,
2.25749633225983));
#37461=CARTESIAN_POINT('Ctrl Pts',(-6.50225495702609,-2.71451482812846,
-0.0364252378376332));
#37462=CARTESIAN_POINT('Ctrl Pts',(-6.3755248784603,-1.44673808137638,-2.29714311133987));
#37463=CARTESIAN_POINT('Ctrl Pts',(-6.24879479989453,1.13982352879828,-2.46388308839495));
#37464=CARTESIAN_POINT('Ctrl Pts',(-6.12206472132875,2.68737051973931,-0.38465210218705));
#37465=CARTESIAN_POINT('Ctrl Pts',(-5.99533464276298,1.78522491637979,2.04521137000987));
#37466=CARTESIAN_POINT('Ctrl Pts',(-5.8686045641972,-0.744255743569043,
2.61074719922196));
#37467=CARTESIAN_POINT('Ctrl Pts',(-5.74187448563141,-2.59530454237517,
0.796436992114019));
#37468=CARTESIAN_POINT('Ctrl Pts',(-5.61514440706564,-2.08058417362054,
-1.74387128153443));
#37469=CARTESIAN_POINT('Ctrl Pts',(-5.48841432849986,0.330708180463282,
-2.69454071215402));
#37470=CARTESIAN_POINT('Ctrl Pts',(-5.36168424993407,2.44054103180832,-1.18898150622322));
#37471=CARTESIAN_POINT('Ctrl Pts',(-5.23495417136831,2.32568054526282,1.40040263905308));
#37472=CARTESIAN_POINT('Ctrl Pts',(-5.10822409280252,0.0908286520274319,
2.71323933814391));
#37473=CARTESIAN_POINT('Ctrl Pts',(-4.98149401423675,-2.22681877483003,
1.55280252902471));
#37474=CARTESIAN_POINT('Ctrl Pts',(-4.85476393567096,-2.51459297747725,
-1.02310298000874));
#37475=CARTESIAN_POINT('Ctrl Pts',(-4.72803385710519,-0.510171240130598,
-2.66639135458844));
#37476=CARTESIAN_POINT('Ctrl Pts',(-4.60130377853941,1.95930088740016,-1.87911084896963));
#37477=CARTESIAN_POINT('Ctrl Pts',(-4.47457369997363,2.64275771163805,0.621087133707496));
#37478=CARTESIAN_POINT('Ctrl Pts',(-4.34784362140786,0.917189078770414,
2.55512851807153));
#37479=CARTESIAN_POINT('Ctrl Pts',(-4.22111354284207,-1.64445008376195,
2.16002348878593));
#37480=CARTESIAN_POINT('Ctrl Pts',(-4.0943834642763,-2.7070785358948,-0.20406702469015));
#37481=CARTESIAN_POINT('Ctrl Pts',(-3.96765338571052,-1.3020494049599,-2.38213872331384));
#37482=CARTESIAN_POINT('Ctrl Pts',(-3.84092330714474,1.28987254978213,-2.3887541429524));
#37483=CARTESIAN_POINT('Ctrl Pts',(-3.71419322857896,2.70600158364826,-0.21788294855305));
#37484=CARTESIAN_POINT('Ctrl Pts',(-3.58746315001318,1.65545473833367,2.15160106882283));
#37485=CARTESIAN_POINT('Ctrl Pts',(-3.4607330714474,-0.904134192255527,
2.55977712173459));
#37486=CARTESIAN_POINT('Ctrl Pts',(-3.33400299288163,-2.63955287190295,
0.634569291483229));
#37487=CARTESIAN_POINT('Ctrl Pts',(-3.20727291431585,-1.96886749038081,
-1.86908489784414));
#37488=CARTESIAN_POINT('Ctrl Pts',(-3.08054283575007,0.496553703384974,
-2.66896084137883));
#37489=CARTESIAN_POINT('Ctrl Pts',(-2.95381275718429,2.50933767235691,-1.03592566817167));
#37490=CARTESIAN_POINT('Ctrl Pts',(-2.82708267861852,2.23471621679757,1.54141525298257));
#37491=CARTESIAN_POINT('Ctrl Pts',(-2.70035260005273,-0.0769774406359214,
2.7136676367567));
#37492=CARTESIAN_POINT('Ctrl Pts',(-2.57362252148696,-2.31850172844312,
1.41225608147515));
#37493=CARTESIAN_POINT('Ctrl Pts',(-2.44689244292118,-2.44657853407578,
-1.17650799064241));
#37494=CARTESIAN_POINT('Ctrl Pts',(-2.3201623643554,-0.344458432372982,
-2.69281749319986));
#37495=CARTESIAN_POINT('Ctrl Pts',(-2.19343228578962,2.07165524152565,-1.75446908867248));
#37496=CARTESIAN_POINT('Ctrl Pts',(-2.06670220722384,2.59933630757378,0.783178509443182));
#37497=CARTESIAN_POINT('Ctrl Pts',(-1.93997212865807,0.757572747850102,
2.60691421348924));
#37498=CARTESIAN_POINT('Ctrl Pts',(-1.81324205009229,-1.77476136749129,
2.05429728834587));
#37499=CARTESIAN_POINT('Ctrl Pts',(-1.68651197152651,-2.68929954337174,
-0.370928511204314));
#37500=CARTESIAN_POINT('Ctrl Pts',(-1.55978189296073,-1.15238481895627,
-2.45803377332412));
#37501=CARTESIAN_POINT('Ctrl Pts',(-1.43305181439495,1.43499125810976,-2.30449604112431));
#37502=CARTESIAN_POINT('Ctrl Pts',(-1.30632173582917,2.71429724812692,-0.0502854555507226));
#37503=CARTESIAN_POINT('Ctrl Pts',(-1.17959165726339,1.51935228042046,2.24977781891539));
#37504=CARTESIAN_POINT('Ctrl Pts',(-1.05286157869761,-1.0605445781299,2.49901152802161));
#37505=CARTESIAN_POINT('Ctrl Pts',(-0.926131500131838,-2.67374177776255,
0.470305794192473));
#37506=CARTESIAN_POINT('Ctrl Pts',(-0.799401421566061,-1.8495789194059,
-1.98721195719532));
#37507=CARTESIAN_POINT('Ctrl Pts',(-0.67267134300028,0.660408141737237,
-2.63307875489731));
#37508=CARTESIAN_POINT('Ctrl Pts',(-0.545941264434503,2.56872557413171,
-0.879111277712124));
#37509=CARTESIAN_POINT('Ctrl Pts',(-0.419211185868724,2.13487199941306,
1.67691920253741));
#37510=CARTESIAN_POINT('Ctrl Pts',(-0.292481107302946,-0.243836522471383,
2.70299842755841));
#37511=CARTESIAN_POINT('Ctrl Pts',(-0.165751028737168,-2.4025868511699,
1.26773016517814));
#37512=CARTESIAN_POINT('Ctrl Pts',(-0.0390209501713873,-2.36667404855317,
-1.32834698267222));
#37513=CARTESIAN_POINT('Ctrl Pts',(0.0454657688724642,-0.91121953791458,
-2.24382588725992));
#37514=CARTESIAN_POINT('Ctrl Pts',(0.0877091283943902,-0.150229390527176,
-2.29366877959735));
#37515=CARTESIAN_POINT('Ctrl Pts',(-11.7372091283944,1.24871913126437,-1.74610375092436));
#37516=CARTESIAN_POINT('Ctrl Pts',(-11.6949657688725,1.82803893654284,-1.33180550341839));
#37517=CARTESIAN_POINT('Ctrl Pts',(-11.6104790498286,2.53215449452145,0.111382902693765));
#37518=CARTESIAN_POINT('Ctrl Pts',(-11.4837489712628,1.28222402163311,2.18912027470234));
#37519=CARTESIAN_POINT('Ctrl Pts',(-11.3570188926971,-1.13759076443305,
2.26497332005167));
#37520=CARTESIAN_POINT('Ctrl Pts',(-11.2302888141313,-2.51986680731908,
0.279367911118224));
#37521=CARTESIAN_POINT('Ctrl Pts',(-11.1035587355655,-1.60543313290645,
-1.96255582577224));
#37522=CARTESIAN_POINT('Ctrl Pts',(-10.9768286569997,0.772599075857153,
-2.41462939592159));
#37523=CARTESIAN_POINT('Ctrl Pts',(-10.850098578434,2.44628207208438,-0.666084462251818));
#37524=CARTESIAN_POINT('Ctrl Pts',(-10.7233684998682,1.8900808053082,1.68987325821547));
#37525=CARTESIAN_POINT('Ctrl Pts',(-10.5966384213024,-0.389059900876383,
2.50528933813506));
#37526=CARTESIAN_POINT('Ctrl Pts',(-10.4699083427366,-2.31353850777508,
1.03705588610104));
#37527=CARTESIAN_POINT('Ctrl Pts',(-10.3431782641708,-2.12909998322721,
-1.37654798263025));
#37528=CARTESIAN_POINT('Ctrl Pts',(-10.2164481856051,-0.00386132140892683,
-2.53533125024933));
#37529=CARTESIAN_POINT('Ctrl Pts',(-10.0897181070393,2.1248954759936,-1.38302391435088));
#37530=CARTESIAN_POINT('Ctrl Pts',(-9.96298802847351,2.31668887208617,1.02999412491035));
#37531=CARTESIAN_POINT('Ctrl Pts',(-9.8362579499077,0.396686825823557,2.50411075248815));
#37532=CARTESIAN_POINT('Ctrl Pts',(-9.70952787134194,-1.88491780588221,
1.69558795529358));
#37533=CARTESIAN_POINT('Ctrl Pts',(-9.58279779277616,-2.44831171288684,
-0.658561375497717));
#37534=CARTESIAN_POINT('Ctrl Pts',(-9.45606771421038,-0.779928793163236,
-2.41239380858159));
#37535=CARTESIAN_POINT('Ctrl Pts',(-9.32933763564459,1.59940398653894,-1.9671909114524));
#37536=CARTESIAN_POINT('Ctrl Pts',(-9.20260755707883,2.52078817930237,0.271219602366674));
#37537=CARTESIAN_POINT('Ctrl Pts',(-9.07587747851304,1.14432914013092,2.26239781531688));
#37538=CARTESIAN_POINT('Ctrl Pts',(-8.94914739994727,-1.27525163676714,
2.19127049335493));
#37539=CARTESIAN_POINT('Ctrl Pts',(-8.82241732138148,-2.5323672975218,0.122674232785287));
#37540=CARTESIAN_POINT('Ctrl Pts',(-8.69568724281572,-1.4810847031977,-2.05774662970121));
#37541=CARTESIAN_POINT('Ctrl Pts',(-8.56895716424991,0.920291672519785,
-2.36241324405171));
#37542=CARTESIAN_POINT('Ctrl Pts',(-8.44222708568416,2.48276932653758,-0.513604484650522));
#37543=CARTESIAN_POINT('Ctrl Pts',(-8.31549700711837,1.78206012617869,1.80338426339693));
#37544=CARTESIAN_POINT('Ctrl Pts',(-8.18876692855259,-0.543099242607164,
2.47648466754675));
#37545=CARTESIAN_POINT('Ctrl Pts',(-8.06203684998681,-2.37319245558576,
0.892127044878068));
#37546=CARTESIAN_POINT('Ctrl Pts',(-7.93530677142103,-2.03998442644912,
-1.50545562380632));
#37547=CARTESIAN_POINT('Ctrl Pts',(-7.80857669285526,0.152786586360089,
-2.53072901642739));
#37548=CARTESIAN_POINT('Ctrl Pts',(-7.68184661428948,2.20628384947819,-1.24909754263459));
#37549=CARTESIAN_POINT('Ctrl Pts',(-7.55511653572371,2.2486266523892,1.17115809080136));
#37550=CARTESIAN_POINT('Ctrl Pts',(-7.42838645715792,0.241217098028255,
2.52383585185799));
#37551=CARTESIAN_POINT('Ctrl Pts',(-7.30165637859215,-1.98607569696558,
1.57589226199505));
#37552=CARTESIAN_POINT('Ctrl Pts',(-7.17492630002637,-2.40294641177284,
-0.808567645681122));
#37553=CARTESIAN_POINT('Ctrl Pts',(-7.04819622146058,-0.629393444329111,
-2.45597169929387));
#37554=CARTESIAN_POINT('Ctrl Pts',(-6.92146614289482,1.71788780068177,-1.86461647524734));
#37555=CARTESIAN_POINT('Ctrl Pts',(-6.79473606432902,2.49921563798099,0.426443771635388));
#37556=CARTESIAN_POINT('Ctrl Pts',(-6.66800598576326,1.00236486352858,2.32877602526715));
#37557=CARTESIAN_POINT('Ctrl Pts',(-6.54127590719748,-1.40819906098522,
2.10829516437708));
#37558=CARTESIAN_POINT('Ctrl Pts',(-6.41454582863168,-2.53510865288725,
-0.0340178416668884));
#37559=CARTESIAN_POINT('Ctrl Pts',(-6.28781575006593,-1.35112108821576,
-2.14532163100879));
#37560=CARTESIAN_POINT('Ctrl Pts',(-6.16108567150013,1.06449095826574,-2.30104152402036));
#37561=CARTESIAN_POINT('Ctrl Pts',(-6.03435559293437,2.50975835074084,-0.359229893497372));
#37562=CARTESIAN_POINT('Ctrl Pts',(-5.90762551436857,1.66723684319845,1.910040419514));
#37563=CARTESIAN_POINT('Ctrl Pts',(-5.78089543580281,-0.695066814862014,
2.43819917528759));
#37564=CARTESIAN_POINT('Ctrl Pts',(-5.65416535723702,-2.42377714576313,
0.743799329908159));
#37565=CARTESIAN_POINT('Ctrl Pts',(-5.52743527867125,-1.94307538384022,
-1.62861632934515));
#37566=CARTESIAN_POINT('Ctrl Pts',(-5.40070520010547,0.308851202868963,
-2.51645465486305));
#37567=CARTESIAN_POINT('Ctrl Pts',(-5.27397512153969,2.27924217740573,-1.11040001451292));
#37568=CARTESIAN_POINT('Ctrl Pts',(-5.14724504297392,2.17197298502593,1.3078480216803));
#37569=CARTESIAN_POINT('Ctrl Pts',(-5.02051496440813,0.0848256562457381,
2.53391746186373));
#37570=CARTESIAN_POINT('Ctrl Pts',(-4.89378488584236,-2.07964513068273,
1.45017558451496));
#37571=CARTESIAN_POINT('Ctrl Pts',(-4.76705480727658,-2.3483999238594,-0.955484637821318));
#37572=CARTESIAN_POINT('Ctrl Pts',(-4.6403247287108,-0.476453291729102,
-2.49016572868064));
#37573=CARTESIAN_POINT('Ctrl Pts',(-4.51359465014502,1.82980788382077,-1.75491771995277));
#37574=CARTESIAN_POINT('Ctrl Pts',(-4.38686457157924,2.46809406706291,0.58003859494274));
#37575=CARTESIAN_POINT('Ctrl Pts',(-4.26013449301346,0.856570738104105,
2.38625641248314));
#37576=CARTESIAN_POINT('Ctrl Pts',(-4.13340441444769,-1.53576602101686,
2.01726444081954));
#37577=CARTESIAN_POINT('Ctrl Pts',(-4.0066743358819,-2.52816383586448,-0.190579942574003));
#37578=CARTESIAN_POINT('Ctrl Pts',(-3.87994425731613,-1.2159950937812,-2.22469976117771));
#37579=CARTESIAN_POINT('Ctrl Pts',(-3.75321417875035,1.20462302441316,-2.23087795825159));
#37580=CARTESIAN_POINT('Ctrl Pts',(-3.62648410018457,2.52715806093534,-0.203482752228769));
#37581=CARTESIAN_POINT('Ctrl Pts',(-3.49975402161879,1.54604336219683,2.00939867066223));
#37582=CARTESIAN_POINT('Ctrl Pts',(-3.37302394305301,-0.84437866774835,
2.39059778326806));
#37583=CARTESIAN_POINT('Ctrl Pts',(-3.24629386448724,-2.46510103977886,
0.592629697589368));
#37584=CARTESIAN_POINT('Ctrl Pts',(-3.11956378592146,-1.83874221630024,
-1.74555439830567));
#37585=CARTESIAN_POINT('Ctrl Pts',(-2.99283370735568,0.463735757502715,
-2.49256539440665));
#37586=CARTESIAN_POINT('Ctrl Pts',(-2.8661036287899,2.343491949386,-0.967459856146969));
#37587=CARTESIAN_POINT('Ctrl Pts',(-2.73937355022413,2.08702061939257,1.43954090986591));
#37588=CARTESIAN_POINT('Ctrl Pts',(-2.61264347165834,-0.0718898912657027,
2.53431745360739));
#37589=CARTESIAN_POINT('Ctrl Pts',(-2.48591339309257,-2.16526862649802,
1.31891805310516));
#37590=CARTESIAN_POINT('Ctrl Pts',(-2.35918331452679,-2.28488065249581,
-1.09875089145302));
#37591=CARTESIAN_POINT('Ctrl Pts',(-2.23245323596101,-0.321692680924034,
-2.51484532591917));
#37592=CARTESIAN_POINT('Ctrl Pts',(-2.10572315739523,1.93473657766382,-1.63851371222139));
#37593=CARTESIAN_POINT('Ctrl Pts',(-1.97899307882946,2.42754244582172,0.731417119358184));
#37594=CARTESIAN_POINT('Ctrl Pts',(-1.85226300026367,0.707503679245126,
2.43461951707511));
#37595=CARTESIAN_POINT('Ctrl Pts',(-1.7255329216979,-1.65746484525164,1.91852583648585));
#37596=CARTESIAN_POINT('Ctrl Pts',(-1.59880284313211,-2.51155988243686,
-0.346413314310394));
#37597=CARTESIAN_POINT('Ctrl Pts',(-1.47207276456634,-1.07622205475522,
-2.2955787985654));
#37598=CARTESIAN_POINT('Ctrl Pts',(-1.34534268600056,1.34015062933357,-2.15218859512606));
#37599=CARTESIAN_POINT('Ctrl Pts',(-1.21861260743479,2.53490545305983,-0.0469620177278084));
#37600=CARTESIAN_POINT('Ctrl Pts',(-1.091882528869,1.41893611077949,2.10108677864122));
#37601=CARTESIAN_POINT('Ctrl Pts',(-0.965152450303225,-0.99045166706401,
2.33384827472851));
#37602=CARTESIAN_POINT('Ctrl Pts',(-0.838422371737447,-2.49703035185308,
0.439222610245357));
#37603=CARTESIAN_POINT('Ctrl Pts',(-0.711692293171671,-1.72733759793698,
-1.855874271013));
#37604=CARTESIAN_POINT('Ctrl Pts',(-0.58496221460589,0.61676082119971,-2.45905480644435));
#37605=CARTESIAN_POINT('Ctrl Pts',(-0.458232136040112,2.39895481962198,
-0.821009553488159));
#37606=CARTESIAN_POINT('Ctrl Pts',(-0.331502057474334,1.99377524942465,
1.56608920920002));
#37607=CARTESIAN_POINT('Ctrl Pts',(-0.204771978908555,-0.227721017252045,
2.52435338773536));
#37608=CARTESIAN_POINT('Ctrl Pts',(-0.0780419003427782,-2.24379644295895,
1.18394406174051));
#37609=CARTESIAN_POINT('Ctrl Pts',(0.048688178223003,-2.21025716893482,
-1.24055462689471));
#37610=CARTESIAN_POINT('Ctrl Pts',(0.133174897266854,-0.850995732758557,
-2.09552821867874));
#37611=CARTESIAN_POINT('Ctrl Pts',(0.17541825678878,-0.140300514809111,
-2.14207692283029));
#37612=CARTESIAN_POINT('Ctrl Pts',(-11.6495,1.16034898466908,-1.62253437445172));
#37613=CARTESIAN_POINT('Ctrl Pts',(-11.6072566404781,1.69867111894511,-1.23755544779991));
#37614=CARTESIAN_POINT('Ctrl Pts',(-11.5227699214342,2.35295738103105,0.103500486870383));
#37615=CARTESIAN_POINT('Ctrl Pts',(-11.3960398428684,1.19148277972948,2.03419922420614));
#37616=CARTESIAN_POINT('Ctrl Pts',(-11.2693097643027,-1.05708502050599,
2.10468425318621));
#37617=CARTESIAN_POINT('Ctrl Pts',(-11.1425796857369,-2.34153927666138,
0.259597425793341));
#37618=CARTESIAN_POINT('Ctrl Pts',(-11.0158496071711,-1.49181882385021,
-1.82366843173565));
#37619=CARTESIAN_POINT('Ctrl Pts',(-10.8891195286053,0.717923294984202,
-2.24374937306581));
#37620=CARTESIAN_POINT('Ctrl Pts',(-10.7623894500395,2.27316203258867,-0.618946575035767));
#37621=CARTESIAN_POINT('Ctrl Pts',(-10.6356593714738,1.75632236943564,1.57028323687515));
#37622=CARTESIAN_POINT('Ctrl Pts',(-10.508929292908,-0.361526663326025,
2.32799343505198));
#37623=CARTESIAN_POINT('Ctrl Pts',(-10.3821992143422,-2.14981254893681,
0.963664858136657));
#37624=CARTESIAN_POINT('Ctrl Pts',(-10.2554691357764,-1.97842648674338,
-1.27913156289677));
#37625=CARTESIAN_POINT('Ctrl Pts',(-10.1287390572107,-0.00358806096914,
-2.35590932209698));
#37626=CARTESIAN_POINT('Ctrl Pts',(-10.0020089786449,1.97451952674142,-1.2851492017786));
#37627=CARTESIAN_POINT('Ctrl Pts',(-9.8752789000791,2.15273996627044,0.957102848135853));
#37628=CARTESIAN_POINT('Ctrl Pts',(-9.74854882151332,0.368613841216539,
2.32689825630081));
#37629=CARTESIAN_POINT('Ctrl Pts',(-9.62181874294755,-1.75152474842402,
1.57559351264993));
#37630=CARTESIAN_POINT('Ctrl Pts',(-9.49508866438176,-2.27504803848494,
-0.611955886851293));
#37631=CARTESIAN_POINT('Ctrl Pts',(-9.368358585816,-0.724734298212267,-2.24167199518702));
#37632=CARTESIAN_POINT('Ctrl Pts',(-9.2416285072502,1.48621635193257,-1.82797549873587));
#37633=CARTESIAN_POINT('Ctrl Pts',(-9.11489842868443,2.34239544440841,0.252025761717839));
#37634=CARTESIAN_POINT('Ctrl Pts',(-8.98816835011866,1.06334653056341,2.10229101340218));
#37635=CARTESIAN_POINT('Ctrl Pts',(-8.86143827155287,-1.18500382101302,
2.03619727482286));
#37636=CARTESIAN_POINT('Ctrl Pts',(-8.7347081929871,-2.35315512425386,0.113992744960442));
#37637=CARTESIAN_POINT('Ctrl Pts',(-8.60797811442132,-1.37627036259484,
-1.91212271254496));
#37638=CARTESIAN_POINT('Ctrl Pts',(-8.48124803585554,0.85516388839699,-2.19522848691248));
#37639=CARTESIAN_POINT('Ctrl Pts',(-8.35451795728975,2.30706713390257,-0.47725739709158));
#37640=CARTESIAN_POINT('Ctrl Pts',(-8.22778787872399,1.65594616616223,1.67576122332812));
#37641=CARTESIAN_POINT('Ctrl Pts',(-8.10105780015819,-0.504664851331058,
2.30122723164079));
#37642=CARTESIAN_POINT('Ctrl Pts',(-7.97432772159243,-2.20524486837564,
0.828992432967621));
#37643=CARTESIAN_POINT('Ctrl Pts',(-7.84759764302665,-1.89561751614567,
-1.39891658645389));
#37644=CARTESIAN_POINT('Ctrl Pts',(-7.72086756446086,0.141974088420104,
-2.35163278207385));
#37645=CARTESIAN_POINT('Ctrl Pts',(-7.5941374858951,2.05014815624844,-1.16070061638369));
#37646=CARTESIAN_POINT('Ctrl Pts',(-7.46740740732931,2.08949441685714,1.08827683305561));
#37647=CARTESIAN_POINT('Ctrl Pts',(-7.34067732876354,0.224146493614207,
2.3452274373418));
#37648=CARTESIAN_POINT('Ctrl Pts',(-7.21394725019775,-1.84552383378359,
1.4643685200068));
#37649=CARTESIAN_POINT('Ctrl Pts',(-7.08721717163198,-2.23289317774092,
-0.75134641827133));
#37650=CARTESIAN_POINT('Ctrl Pts',(-6.96048709306619,-0.584852130314656,
-2.28216593812101));
#37651=CARTESIAN_POINT('Ctrl Pts',(-6.83375701450043,1.59631522845185,-1.73266011521722));
#37652=CARTESIAN_POINT('Ctrl Pts',(-6.70702693593464,2.32234956235835,0.396264928634968));
#37653=CARTESIAN_POINT('Ctrl Pts',(-6.58029685736886,0.931428871827763,
2.16397172813741));
#37654=CARTESIAN_POINT('Ctrl Pts',(-6.45356677880309,-1.30854273768647,
1.95909399649433));
#37655=CARTESIAN_POINT('Ctrl Pts',(-6.3268367002373,-2.35570247764605,-0.03161044549615));
#37656=CARTESIAN_POINT('Ctrl Pts',(-6.20010662167154,-1.25550409505514,
-1.9935001506777));
#37657=CARTESIAN_POINT('Ctrl Pts',(-6.07337654310573,0.989158387733211,
-2.13819995964578));
#37658=CARTESIAN_POINT('Ctrl Pts',(-5.94664646453999,2.33214618174238,-0.333807684807691));
#37659=CARTESIAN_POINT('Ctrl Pts',(-5.81991638597417,1.54924877001712,1.77486946901812));
#37660=CARTESIAN_POINT('Ctrl Pts',(-5.69318630740843,-0.645877886154986,
2.26565115135322));
#37661=CARTESIAN_POINT('Ctrl Pts',(-5.56645622884262,-2.25224974915109,
0.691161667702299));
#37662=CARTESIAN_POINT('Ctrl Pts',(-5.43972615027687,-1.8055665940599,-1.51336137715587));
#37663=CARTESIAN_POINT('Ctrl Pts',(-5.31299607171107,0.286994225274642,
-2.33836859757207));
#37664=CARTESIAN_POINT('Ctrl Pts',(-5.18626599314531,2.11794332300315,-1.03181852280261));
#37665=CARTESIAN_POINT('Ctrl Pts',(-5.05953591457952,2.01826542478903,1.21529340430752));
#37666=CARTESIAN_POINT('Ctrl Pts',(-4.93280583601374,0.0788226604640474,
2.35459558558354));
#37667=CARTESIAN_POINT('Ctrl Pts',(-4.80607575744796,-1.93247148653543,
1.34754864000521));
#37668=CARTESIAN_POINT('Ctrl Pts',(-4.67934567888219,-2.18220687024155,
-0.887866295633901));
#37669=CARTESIAN_POINT('Ctrl Pts',(-4.55261560031641,-0.442735343327605,
-2.31394010277285));
#37670=CARTESIAN_POINT('Ctrl Pts',(-4.42588552175063,1.70031488024139,-1.63072459093592));
#37671=CARTESIAN_POINT('Ctrl Pts',(-4.29915544318485,2.29343042248776,0.538990056177979));
#37672=CARTESIAN_POINT('Ctrl Pts',(-4.17242536461907,0.795952397437793,
2.21738430689477));
#37673=CARTESIAN_POINT('Ctrl Pts',(-4.0456952860533,-1.42708195827177,1.87450539285314));
#37674=CARTESIAN_POINT('Ctrl Pts',(-3.91896520748751,-2.34924913583417,
-0.177092860457853));
#37675=CARTESIAN_POINT('Ctrl Pts',(-3.79223512892175,-1.12994078260249,
-2.06726079904157));
#37676=CARTESIAN_POINT('Ctrl Pts',(-3.66550505035595,1.11937349904418,-2.07300177355078));
#37677=CARTESIAN_POINT('Ctrl Pts',(-3.53877497179019,2.34831453822241,-0.189082555904491));
#37678=CARTESIAN_POINT('Ctrl Pts',(-3.4120448932244,1.43663198605998,1.86719627250164));
#37679=CARTESIAN_POINT('Ctrl Pts',(-3.28531481465863,-0.784623143241175,
2.22141844480153));
#37680=CARTESIAN_POINT('Ctrl Pts',(-3.15858473609284,-2.29064920765476,
0.55069010369551));
#37681=CARTESIAN_POINT('Ctrl Pts',(-3.03185465752707,-1.70861694221966,
-1.6220238987672));
#37682=CARTESIAN_POINT('Ctrl Pts',(-2.90512457896129,0.430917811620456,
-2.31616994743447));
#37683=CARTESIAN_POINT('Ctrl Pts',(-2.77839450039551,2.1776462264151,-0.898994044122268));
#37684=CARTESIAN_POINT('Ctrl Pts',(-2.65166442182973,1.93932502198757,1.33766656674925));
#37685=CARTESIAN_POINT('Ctrl Pts',(-2.52493434326395,-0.066802341895476,
2.35496727045807));
#37686=CARTESIAN_POINT('Ctrl Pts',(-2.39820426469818,-2.01203552455293,
1.22558002473516));
#37687=CARTESIAN_POINT('Ctrl Pts',(-2.2714741861324,-2.12318277091584,-1.02099379226364));
#37688=CARTESIAN_POINT('Ctrl Pts',(-2.14474410756662,-0.298926929475087,
-2.33687315863848));
#37689=CARTESIAN_POINT('Ctrl Pts',(-2.01801402900084,1.79781791380199,-1.52255833577031));
#37690=CARTESIAN_POINT('Ctrl Pts',(-1.89128395043506,2.25574858406966,0.679655729273182));
#37691=CARTESIAN_POINT('Ctrl Pts',(-1.76455387186929,0.657434610640146,
2.26232482066099));
#37692=CARTESIAN_POINT('Ctrl Pts',(-1.6378237933035,-1.54016832301198,1.78275438462583));
#37693=CARTESIAN_POINT('Ctrl Pts',(-1.51109371473773,-2.33382022150199,
-0.321898117416469));
#37694=CARTESIAN_POINT('Ctrl Pts',(-1.38436363617195,-1.00005929055416,
-2.13312382380668));
#37695=CARTESIAN_POINT('Ctrl Pts',(-1.25763355760617,1.24531000055737,-1.9998811491278));
#37696=CARTESIAN_POINT('Ctrl Pts',(-1.13090347904039,2.35551365799275,-0.0436385799048972));
#37697=CARTESIAN_POINT('Ctrl Pts',(-1.00417340047461,1.31851994113852,1.95239573836704));
#37698=CARTESIAN_POINT('Ctrl Pts',(-0.877443321908835,-0.920358755998121,
2.16868502143541));
#37699=CARTESIAN_POINT('Ctrl Pts',(-0.750713243343058,-2.32031892594361,
0.408139426298241));
#37700=CARTESIAN_POINT('Ctrl Pts',(-0.62398316477728,-1.60509627646806,
-1.72453658483069));
#37701=CARTESIAN_POINT('Ctrl Pts',(-0.497253086211501,0.573113500662185,
-2.2850308579914));
#37702=CARTESIAN_POINT('Ctrl Pts',(-0.370523007645721,2.22918406511225,
-0.762907829264197));
#37703=CARTESIAN_POINT('Ctrl Pts',(-0.243792929079945,1.85267849943624,
1.45525921586262));
#37704=CARTESIAN_POINT('Ctrl Pts',(-0.117062850514165,-0.211605512032712,
2.34570834791232));
#37705=CARTESIAN_POINT('Ctrl Pts',(0.0096672280516118,-2.085006034748,1.10015795830288));
#37706=CARTESIAN_POINT('Ctrl Pts',(0.136397306617393,-2.05384028931649,
-1.1527622711172));
#37707=CARTESIAN_POINT('Ctrl Pts',(0.220884025661244,-0.790771927602532,
-1.94723055009756));
#37708=CARTESIAN_POINT('Ctrl Pts',(0.263127385183171,-0.130371639091046,
-1.99048506606322));
#37709=CARTESIAN_POINT('',(0.,-0.160158266245241,-2.44526063636442));
#37710=CARTESIAN_POINT('Ctrl Pts',(-7.21644966006352E-16,-1.69189910824764,
1.06268379792867));
#37711=CARTESIAN_POINT('Ctrl Pts',(-7.21076027123798E-16,-1.72378408803524,
1.02301469480698));
#37712=CARTESIAN_POINT('Ctrl Pts',(-9.55233987476986E-16,-1.7539898143595,
0.98212740444666));
#37713=CARTESIAN_POINT('Ctrl Pts',(-7.7715611723761E-16,-1.78241555186685,
0.940088493339687));
#37714=CARTESIAN_POINT('Ctrl Pts',(-5.26309397071712E-16,-1.82258537863282,
0.880681212309237));
#37715=CARTESIAN_POINT('Ctrl Pts',(-3.25548323645293E-15,-1.8592027471497,
0.818975806660995));
#37716=CARTESIAN_POINT('Ctrl Pts',(-3.94129173741931E-15,-1.89232248273639,
0.755320817406468));
#37717=CARTESIAN_POINT('Ctrl Pts',(-4.33727841913663E-15,-1.91144585927058,
0.718566347413557));
#37718=CARTESIAN_POINT('Ctrl Pts',(-2.02180909249841E-15,-1.92940249600458,
0.681161140715259));
#37719=CARTESIAN_POINT('Ctrl Pts',(-1.94289029309402E-15,-1.94619730424733,
0.643167074871445));
#37720=CARTESIAN_POINT('Ctrl Pts',(-1.91494498717367E-15,-1.95214437969399,
0.629713299583723));
#37721=CARTESIAN_POINT('Ctrl Pts',(-2.14700471816057E-15,-1.95794660868843,
0.61618355001508));
#37722=CARTESIAN_POINT('Ctrl Pts',(-1.99840144432528E-15,-1.96360123760218,
0.60258734758215));
#37723=CARTESIAN_POINT('Ctrl Pts',(-1.24294016579427E-15,-1.99234793394707,
0.533467709716482));
#37724=CARTESIAN_POINT('Ctrl Pts',(-2.63660178728452E-15,-2.01723098981382,
0.46276284494659));
#37725=CARTESIAN_POINT('Ctrl Pts',(-2.60902410786912E-15,-2.03831315006211,
0.390854522909893));
#37726=CARTESIAN_POINT('Ctrl Pts',(-2.58580080554436E-15,-2.05606654307716,
0.330300163815003));
#37727=CARTESIAN_POINT('Ctrl Pts',(-2.83510209010142E-15,-2.07112396733743,
0.268891343741576));
#37728=CARTESIAN_POINT('Ctrl Pts',(-3.88578058618805E-15,-2.08350029900009,
0.206838312286158));
#37729=CARTESIAN_POINT('Ctrl Pts',(-4.39213530033574E-15,-2.08946483896602,
0.176933022398113));
#37730=CARTESIAN_POINT('Ctrl Pts',(2.96323789960187E-15,-2.0948063589925,
0.146877908022072));
#37731=CARTESIAN_POINT('Ctrl Pts',(3.05311331771918E-15,-2.09952471759412,
0.116695578438766));
#37732=CARTESIAN_POINT('Ctrl Pts',(3.09419245965773E-15,-2.10168132645084,
0.102900213399458));
#37733=CARTESIAN_POINT('Ctrl Pts',(-1.34143688527772E-15,-2.10370806138866,
0.0890758412722826));
#37734=CARTESIAN_POINT('Ctrl Pts',(-1.41553435639707E-15,-2.10560375301678,
0.0752325061236768));
#37735=CARTESIAN_POINT('Ctrl Pts',(-1.82703970662702E-15,-2.11613160552745,
-0.00164739804338759));
#37736=CARTESIAN_POINT('Ctrl Pts',(7.37197929993521E-17,-2.12259963218265,
-0.0789404011946104));
#37737=CARTESIAN_POINT('Ctrl Pts',(-3.88578058618805E-16,-2.12506850073416,
-0.156260019712051));
#37738=CARTESIAN_POINT('Ctrl Pts',(-8.67997835351761E-16,-2.12762880769991,
-0.236443291420884));
#37739=CARTESIAN_POINT('Ctrl Pts',(-6.93190692512345E-16,-2.12588873988702,
-0.316656112225985));
#37740=CARTESIAN_POINT('Ctrl Pts',(-1.38777878078145E-16,-2.1198657520015,
-0.396494553741407));
#37741=CARTESIAN_POINT('Ctrl Pts',(2.77031732747506E-16,-2.11534851108737,
-0.456373384877974));
#37742=CARTESIAN_POINT('Ctrl Pts',(6.39606772428307E-16,-2.10842110187479,
-0.51604230937309));
#37743=CARTESIAN_POINT('Ctrl Pts',(4.44089209850063E-16,-2.09907092634396,
-0.575335244944601));
#37744=CARTESIAN_POINT('Ctrl Pts',(2.97451037916379E-16,-2.09205829469584,
-0.619804946623235));
#37745=CARTESIAN_POINT('Ctrl Pts',(-8.03907321812597E-16,-2.08368251007437,
-0.664063249538941));
#37746=CARTESIAN_POINT('Ctrl Pts',(-8.04911692853238E-16,-2.07393163616088,
-0.708039858350645));
#37747=CARTESIAN_POINT('Ctrl Pts',(-8.05227535616264E-16,-2.07086529629828,
-0.721869103792363));
#37748=CARTESIAN_POINT('Ctrl Pts',(-1.27292777763199E-15,-2.06766293040564,
-0.735670486093707));
#37749=CARTESIAN_POINT('Ctrl Pts',(-1.30451205393456E-15,-2.06432404759794,
-0.749441796406119));
#37750=CARTESIAN_POINT('Ctrl Pts',(-1.33155230346768E-15,-2.06146552953607,
-0.761231829639062));
#37751=CARTESIAN_POINT('Ctrl Pts',(-1.31834190104063E-15,-2.05850921748488,
-0.772990451522471));
#37752=CARTESIAN_POINT('Ctrl Pts',(-1.33226762955019E-15,-2.05545538714023,
-0.784715877967114));
#37753=CARTESIAN_POINT('Ctrl Pts',(-1.42537956622108E-15,-2.03503648715523,
-0.863115881514751));
#37754=CARTESIAN_POINT('Ctrl Pts',(-1.25530095348547E-15,-2.0102604516796,
-0.940037252301371));
#37755=CARTESIAN_POINT('Ctrl Pts',(-9.71445146547012E-16,-1.98114950952945,
-1.0150831509489));
#37756=CARTESIAN_POINT('Ctrl Pts',(-8.74282698905283E-16,-1.97118497710373,
-1.04077099322598));
#37757=CARTESIAN_POINT('Ctrl Pts',(-7.76969050075519E-16,-1.96071209936315,
-1.06623917638337));
#37758=CARTESIAN_POINT('Ctrl Pts',(-8.32667268468867E-16,-1.94973036890473,
-1.09147191710966));
#37759=CARTESIAN_POINT('Ctrl Pts',(-1.01672237405949E-15,-1.91874143595192,
-1.16267524098863));
#37760=CARTESIAN_POINT('Ctrl Pts',(3.52175838536202E-15,-1.88370440096443,
-1.23200476678311));
#37761=CARTESIAN_POINT('Ctrl Pts',(4.91273688396632E-15,-1.84492953449254,
-1.29931700254966));
#37762=CARTESIAN_POINT('Ctrl Pts',(6.33247345622073E-15,-1.80535300899651,
-1.3680208991044));
#37763=CARTESIAN_POINT('Ctrl Pts',(2.18326834371925E-15,-1.76188209226263,
-1.43462390096206));
#37764=CARTESIAN_POINT('Ctrl Pts',(3.24740234702858E-15,-1.71479611157841,
-1.49895472013064));
#37765=CARTESIAN_POINT('Ctrl Pts',(3.50550449537181E-15,-1.7033755642285,
-1.51455794545795));
#37766=CARTESIAN_POINT('Ctrl Pts',(9.82688432106508E-17,-1.69173782534689,
-1.53003274288333));
#37767=CARTESIAN_POINT('Ctrl Pts',(4.16333634234434E-17,-1.67990922204288,
-1.54534767673703));
#37768=CARTESIAN_POINT('Ctrl Pts',(-1.9522263401941E-16,-1.63044066197322,
-1.60939646642361));
#37769=CARTESIAN_POINT('Ctrl Pts',(4.54908001959739E-16,-1.57758717960021,
-1.67072511626626));
#37770=CARTESIAN_POINT('Ctrl Pts',(6.80011602582908E-16,-1.52170661356515,
-1.72918893837752));
#37771=CARTESIAN_POINT('Ctrl Pts',(9.09600338458483E-16,-1.46471264065452,
-1.78881763812208));
#37772=CARTESIAN_POINT('Ctrl Pts',(6.75097762342671E-16,-1.40456926783563,
-1.84546690259517));
#37773=CARTESIAN_POINT('Ctrl Pts',(3.19189119579733E-16,-1.34160425438441,
-1.89896385868516));
#37774=CARTESIAN_POINT('Ctrl Pts',(-3.94837766702072E-17,-1.27815020740864,
-1.95287631226424));
#37775=CARTESIAN_POINT('Ctrl Pts',(-7.23779732573461E-16,-1.21182987269852,
-2.00358802360937));
#37776=CARTESIAN_POINT('Ctrl Pts',(-4.44089209850063E-16,-1.14293528572537,
-2.05089189769593));
#37777=CARTESIAN_POINT('Ctrl Pts',(-3.25410331228778E-16,-1.11370178776685,
-2.07096397835269));
#37778=CARTESIAN_POINT('Ctrl Pts',(1.70065938854078E-15,-1.08400432332864,
-2.09042204748417));
#37779=CARTESIAN_POINT('Ctrl Pts',(1.70696790036118E-15,-1.05386331486469,
-2.1092481624567));
#37780=CARTESIAN_POINT('Ctrl Pts',(1.7101456789279E-15,-1.03868042333605,
-2.11873141720165));
#37781=CARTESIAN_POINT('Ctrl Pts',(-3.82184296166841E-15,-1.02338072840275,
-2.12805668641633));
#37782=CARTESIAN_POINT('Ctrl Pts',(-3.65679708735911E-15,-1.0079928489119,
-2.13720641506556));
#37783=CARTESIAN_POINT('Ctrl Pts',(-2.86527130671852E-15,-0.934195770509449,
-2.18108661590086));
#37784=CARTESIAN_POINT('Ctrl Pts',(2.35760061415838E-15,-0.858275193167998,
-2.22099636818658));
#37785=CARTESIAN_POINT('Ctrl Pts',(2.26901830657766E-15,-0.780581187603902,
-2.25675949833411));
#37786=CARTESIAN_POINT('Ctrl Pts',(2.18029069254155E-15,-0.702759736268041,
-2.29258129272077));
#37787=CARTESIAN_POINT('Ctrl Pts',(9.81873011222773E-16,-0.623158277772009,
-2.32424355037343));
#37788=CARTESIAN_POINT('Ctrl Pts',(1.47798440153224E-15,-0.542089661797717,
-2.35153447222983));
#37789=CARTESIAN_POINT('Ctrl Pts',(1.96365420303237E-15,-0.46272728593377,
-2.37825100577382));
#37790=CARTESIAN_POINT('Ctrl Pts',(-4.5803513406731E-15,-0.381958046000184,
-2.40077878705499));
#37791=CARTESIAN_POINT('Ctrl Pts',(-5.32473370951081E-15,-0.300049960212024,
-2.41887709197029));
#37792=CARTESIAN_POINT('Ctrl Pts',(-5.74534480860178E-15,-0.253768033839171,
-2.42910348668461));
#37793=CARTESIAN_POINT('Ctrl Pts',(-1.31935727443843E-16,-0.20712210076169,
-2.43791483968498));
#37794=CARTESIAN_POINT('Ctrl Pts',(0.,-0.160158266245241,-2.44526063636442));
#37795=CARTESIAN_POINT('Ctrl Pts',(0.,-0.160158266245241,-2.44526063636442));
#37796=CARTESIAN_POINT('Ctrl Pts',(-0.0422433595219261,-0.971443343070605,
-2.3921235558411));
#37797=CARTESIAN_POINT('Ctrl Pts',(-0.0844867190438518,-1.74726713562105,
-1.90413144714542));
#37798=CARTESIAN_POINT('Ctrl Pts',(-0.126730078565778,-2.14156008709783,
-1.19885945828666));
#37799=CARTESIAN_POINT('Ctrl Pts',(-0.148377553639829,-2.34361425455905,
-0.83744507335068));
#37800=CARTESIAN_POINT('Ctrl Pts',(-0.17002502871388,-2.44547775967852,
-0.418972614037773));
#37801=CARTESIAN_POINT('Ctrl Pts',(-0.191672503787931,-2.44601738174545,
-0.0004368899209653));
#37802=CARTESIAN_POINT('Origin',(0.6,4.98642551413971,-0.829870828464581));
#37803=CARTESIAN_POINT('',(7.6,4.69510848352227,-0.997976115925247));
#37804=CARTESIAN_POINT('',(7.4,4.92450311121048,-0.865603320048102));
#37805=CARTESIAN_POINT('Ctrl Pts',(7.6,4.69510848352227,-0.997976115925247));
#37806=CARTESIAN_POINT('Ctrl Pts',(7.50357879858669,4.80746503585943,-0.9331404608017));
#37807=CARTESIAN_POINT('Ctrl Pts',(7.4,4.92450311121048,-0.8656033200481));
#37808=CARTESIAN_POINT('',(0.6,4.69510848352227,-0.997976115925247));
#37809=CARTESIAN_POINT('',(0.6,4.69510848352227,-0.997976115925247));
#37810=CARTESIAN_POINT('',(0.6,4.92450311121048,-0.865603320048101));
#37811=CARTESIAN_POINT('',(0.6,4.98642551413971,-0.829870828464581));
#37812=CARTESIAN_POINT('',(3.95,4.92450311121048,-0.865603320048102));
#37813=CARTESIAN_POINT('Origin',(0.6,4.81737693361399,-1.02396507727747));
#37814=CARTESIAN_POINT('',(0.6,4.85083003702482,-1.21220788311979));
#37815=CARTESIAN_POINT('Origin',(0.6,0.,0.));
#37816=CARTESIAN_POINT('',(0.6,4.69510848352227,-0.997976115925247));
#37817=CARTESIAN_POINT('Origin',(0.6,4.69510848352227,-0.997976115925247));
#37818=CARTESIAN_POINT('',(7.4,4.85083003702482,-1.21220788311979));
#37819=CARTESIAN_POINT('Ctrl Pts',(7.4,4.85083003702482,-1.21220788311979));
#37820=CARTESIAN_POINT('Ctrl Pts',(7.50357879858673,4.77138026482966,-1.10290596108179));
#37821=CARTESIAN_POINT('Ctrl Pts',(7.6,4.69510848352227,-0.997976115925248));
#37822=CARTESIAN_POINT('',(3.95,4.85083003702482,-1.21220788311979));
#37823=CARTESIAN_POINT('Origin',(3.95,0.,0.));
#37824=CARTESIAN_POINT('',(7.4,4.63692185318803,-1.87054957898135));
#37825=CARTESIAN_POINT('Origin',(7.4,0.,0.));
#37826=CARTESIAN_POINT('',(0.6,4.63692185318803,-1.87054957898136));
#37827=CARTESIAN_POINT('',(3.95,4.63692185318803,-1.87054957898135));
#37828=CARTESIAN_POINT('',(0.6,4.49279557168125,-2.19426250733164));
#37829=CARTESIAN_POINT('Origin',(0.6,0.,0.));
#37830=CARTESIAN_POINT('',(7.4,4.49279557168125,-2.19426250733164));
#37831=CARTESIAN_POINT('',(3.95,4.49279557168125,-2.19426250733164));
#37832=CARTESIAN_POINT('',(7.4,4.14668485976156,-2.79374384542038));
#37833=CARTESIAN_POINT('Origin',(7.4,0.,0.));
#37834=CARTESIAN_POINT('',(0.6,4.14668485976156,-2.79374384542038));
#37835=CARTESIAN_POINT('',(3.95,4.14668485976156,-2.79374384542038));
#37836=CARTESIAN_POINT('',(0.6,3.93840438103015,-3.08041733073337));
#37837=CARTESIAN_POINT('Origin',(0.6,0.,0.));
#37838=CARTESIAN_POINT('',(7.4,3.93840438103015,-3.08041733073337));
#37839=CARTESIAN_POINT('',(3.95,3.93840438103015,-3.08041733073337));
#37840=CARTESIAN_POINT('',(7.4,3.4752178399619,-3.59483809994421));
#37841=CARTESIAN_POINT('Origin',(7.4,0.,0.));
#37842=CARTESIAN_POINT('',(0.6,3.4752178399619,-3.59483809994421));
#37843=CARTESIAN_POINT('',(3.95,3.4752178399619,-3.59483809994421));
#37844=CARTESIAN_POINT('',(0.6,3.21188602036704,-3.83194313529973));
#37845=CARTESIAN_POINT('Origin',(0.6,0.,0.));
#37846=CARTESIAN_POINT('',(7.4,3.21188602036704,-3.83194313529973));
#37847=CARTESIAN_POINT('',(3.95,3.21188602036704,-3.83194313529973));
#37848=CARTESIAN_POINT('',(7.4,2.65186712461055,-4.23882067955343));
#37849=CARTESIAN_POINT('Origin',(7.4,0.,0.));
#37850=CARTESIAN_POINT('',(0.6,2.65186712461055,-4.23882067955343));
#37851=CARTESIAN_POINT('',(3.95,2.65186712461055,-4.23882067955343));
#37852=CARTESIAN_POINT('',(0.6,2.3449928282748,-4.41599463715025));
#37853=CARTESIAN_POINT('Origin',(0.6,0.,0.));
#37854=CARTESIAN_POINT('',(7.4,2.3449928282748,-4.41599463715025));
#37855=CARTESIAN_POINT('',(3.95,2.3449928282748,-4.41599463715025));
#37856=CARTESIAN_POINT('',(7.4,1.71261709084344,-4.69754645534783));
#37857=CARTESIAN_POINT('Origin',(7.4,0.,0.));
#37858=CARTESIAN_POINT('',(0.6,1.71261709084344,-4.69754645534783));
#37859=CARTESIAN_POINT('',(3.95,1.71261709084344,-4.69754645534783));
#37860=CARTESIAN_POINT('',(0.6,1.37561219706291,-4.807045983064));
#37861=CARTESIAN_POINT('Origin',(0.6,0.,0.));
#37862=CARTESIAN_POINT('',(7.4,1.37561219706291,-4.807045983064));
#37863=CARTESIAN_POINT('',(3.95,1.37561219706291,-4.807045983064));
#37864=CARTESIAN_POINT('',(7.4,0.698517472157875,-4.95096690971472));
#37865=CARTESIAN_POINT('Origin',(7.4,0.,0.));
#37866=CARTESIAN_POINT('',(0.6,0.698517472157875,-4.95096690971472));
#37867=CARTESIAN_POINT('',(3.95,0.698517472157875,-4.95096690971472));
#37868=CARTESIAN_POINT('',(0.6,0.346110711919692,-4.98800635275201));
#37869=CARTESIAN_POINT('Origin',(0.6,0.,0.));
#37870=CARTESIAN_POINT('',(7.4,0.346110711919692,-4.98800635275201));
#37871=CARTESIAN_POINT('',(3.95,0.346110711919692,-4.98800635275201));
#37872=CARTESIAN_POINT('',(7.4,-0.3461107119197,-4.98800635275201));
#37873=CARTESIAN_POINT('Origin',(7.4,0.,0.));
#37874=CARTESIAN_POINT('',(0.6,-0.3461107119197,-4.98800635275201));
#37875=CARTESIAN_POINT('',(3.95,-0.3461107119197,-4.98800635275201));
#37876=CARTESIAN_POINT('',(0.6,-0.698517472157882,-4.95096690971472));
#37877=CARTESIAN_POINT('Origin',(0.6,0.,0.));
#37878=CARTESIAN_POINT('',(7.4,-0.698517472157882,-4.95096690971472));
#37879=CARTESIAN_POINT('',(3.95,-0.698517472157882,-4.95096690971472));
#37880=CARTESIAN_POINT('',(7.4,-1.37561219706292,-4.807045983064));
#37881=CARTESIAN_POINT('Origin',(7.4,0.,0.));
#37882=CARTESIAN_POINT('',(0.6,-1.37561219706292,-4.807045983064));
#37883=CARTESIAN_POINT('',(3.95,-1.37561219706292,-4.807045983064));
#37884=CARTESIAN_POINT('',(0.6,-1.71261709084344,-4.69754645534783));
#37885=CARTESIAN_POINT('Origin',(0.6,0.,0.));
#37886=CARTESIAN_POINT('',(7.4,-1.71261709084344,-4.69754645534783));
#37887=CARTESIAN_POINT('',(3.95,-1.71261709084344,-4.69754645534783));
#37888=CARTESIAN_POINT('',(7.4,-2.34499282827481,-4.41599463715025));
#37889=CARTESIAN_POINT('Origin',(7.4,0.,0.));
#37890=CARTESIAN_POINT('',(0.6,-2.34499282827481,-4.41599463715025));
#37891=CARTESIAN_POINT('',(3.95,-2.34499282827481,-4.41599463715025));
#37892=CARTESIAN_POINT('',(0.6,-2.65186712461056,-4.23882067955342));
#37893=CARTESIAN_POINT('Origin',(0.6,0.,0.));
#37894=CARTESIAN_POINT('',(7.4,-2.65186712461056,-4.23882067955342));
#37895=CARTESIAN_POINT('',(3.95,-2.65186712461056,-4.23882067955342));
#37896=CARTESIAN_POINT('',(7.4,-3.21188602036705,-3.83194313529973));
#37897=CARTESIAN_POINT('Origin',(7.4,0.,0.));
#37898=CARTESIAN_POINT('',(0.6,-3.21188602036705,-3.83194313529973));
#37899=CARTESIAN_POINT('',(3.95,-3.21188602036705,-3.83194313529973));
#37900=CARTESIAN_POINT('',(0.6,-3.47521783996191,-3.59483809994421));
#37901=CARTESIAN_POINT('Origin',(0.6,0.,0.));
#37902=CARTESIAN_POINT('',(7.4,-3.47521783996191,-3.59483809994421));
#37903=CARTESIAN_POINT('',(3.95,-3.47521783996191,-3.59483809994421));
#37904=CARTESIAN_POINT('',(7.4,-3.93840438103015,-3.08041733073337));
#37905=CARTESIAN_POINT('Origin',(7.4,0.,0.));
#37906=CARTESIAN_POINT('',(0.6,-3.93840438103015,-3.08041733073337));
#37907=CARTESIAN_POINT('',(3.95,-3.93840438103015,-3.08041733073337));
#37908=CARTESIAN_POINT('',(0.6,-4.14668485976156,-2.79374384542038));
#37909=CARTESIAN_POINT('Origin',(0.6,0.,0.));
#37910=CARTESIAN_POINT('',(7.4,-4.14668485976156,-2.79374384542038));
#37911=CARTESIAN_POINT('',(3.95,-4.14668485976156,-2.79374384542038));
#37912=CARTESIAN_POINT('',(7.4,-4.49279557168126,-2.19426250733163));
#37913=CARTESIAN_POINT('Origin',(7.4,0.,0.));
#37914=CARTESIAN_POINT('',(0.6,-4.49279557168126,-2.19426250733163));
#37915=CARTESIAN_POINT('',(3.95,-4.49279557168126,-2.19426250733163));
#37916=CARTESIAN_POINT('',(0.6,-4.63692185318803,-1.87054957898135));
#37917=CARTESIAN_POINT('Origin',(0.6,0.,0.));
#37918=CARTESIAN_POINT('',(7.4,-4.63692185318803,-1.87054957898135));
#37919=CARTESIAN_POINT('',(3.95,-4.63692185318803,-1.87054957898135));
#37920=CARTESIAN_POINT('',(7.4,-4.85083003702482,-1.21220788311979));
#37921=CARTESIAN_POINT('Origin',(7.4,0.,0.));
#37922=CARTESIAN_POINT('',(0.6,-4.85083003702482,-1.21220788311979));
#37923=CARTESIAN_POINT('',(3.95,-4.85083003702482,-1.21220788311979));
#37924=CARTESIAN_POINT('',(0.6,-4.92450311121048,-0.865603320048097));
#37925=CARTESIAN_POINT('Origin',(0.6,0.,0.));
#37926=CARTESIAN_POINT('',(7.4,-4.92450311121048,-0.865603320048097));
#37927=CARTESIAN_POINT('',(3.95,-4.92450311121048,-0.865603320048097));
#37928=CARTESIAN_POINT('',(7.4,-4.99685995288536,-0.177173957596823));
#37929=CARTESIAN_POINT('Origin',(7.4,0.,0.));
#37930=CARTESIAN_POINT('',(0.6,-4.99685995288536,-0.177173957596823));
#37931=CARTESIAN_POINT('',(3.95,-4.99685995288536,-0.177173957596823));
#37932=CARTESIAN_POINT('',(0.6,-5.,-6.12323399573677E-16));
#37933=CARTESIAN_POINT('Origin',(0.6,0.,0.));
#37934=CARTESIAN_POINT('',(0.5,-5.,-6.12323399573677E-16));
#37935=CARTESIAN_POINT('',(3.95,-5.,-6.12323399573677E-16));
#37936=CARTESIAN_POINT('Origin',(0.5,0.,0.));
#37937=CARTESIAN_POINT('',(0.6,-4.99685995288536,0.177173957596825));
#37938=CARTESIAN_POINT('Origin',(0.6,0.,0.));
#37939=CARTESIAN_POINT('',(7.4,-4.99685995288536,0.177173957596825));
#37940=CARTESIAN_POINT('',(3.95,-4.99685995288536,0.177173957596825));
#37941=CARTESIAN_POINT('',(7.4,-4.92450311121048,0.865603320048101));
#37942=CARTESIAN_POINT('Origin',(7.4,0.,0.));
#37943=CARTESIAN_POINT('',(0.6,-4.92450311121048,0.865603320048101));
#37944=CARTESIAN_POINT('',(3.95,-4.92450311121048,0.865603320048101));
#37945=CARTESIAN_POINT('',(0.6,-4.85083003702482,1.21220788311979));
#37946=CARTESIAN_POINT('Origin',(0.6,0.,0.));
#37947=CARTESIAN_POINT('',(7.4,-4.85083003702482,1.21220788311979));
#37948=CARTESIAN_POINT('',(3.95,-4.85083003702482,1.21220788311979));
#37949=CARTESIAN_POINT('',(7.4,-4.63692185318803,1.87054957898135));
#37950=CARTESIAN_POINT('Origin',(7.4,0.,0.));
#37951=CARTESIAN_POINT('',(0.6,-4.63692185318803,1.87054957898135));
#37952=CARTESIAN_POINT('',(3.95,-4.63692185318803,1.87054957898135));
#37953=CARTESIAN_POINT('',(0.6,-4.49279557168125,2.19426250733163));
#37954=CARTESIAN_POINT('Origin',(0.6,0.,0.));
#37955=CARTESIAN_POINT('',(7.4,-4.49279557168125,2.19426250733164));
#37956=CARTESIAN_POINT('',(3.95,-4.49279557168125,2.19426250733164));
#37957=CARTESIAN_POINT('',(7.4,-4.14668485976156,2.79374384542038));
#37958=CARTESIAN_POINT('Origin',(7.4,0.,0.));
#37959=CARTESIAN_POINT('',(0.6,-4.14668485976156,2.79374384542038));
#37960=CARTESIAN_POINT('',(3.95,-4.14668485976156,2.79374384542038));
#37961=CARTESIAN_POINT('',(0.6,-3.93840438103015,3.08041733073337));
#37962=CARTESIAN_POINT('Origin',(0.6,0.,0.));
#37963=CARTESIAN_POINT('',(7.4,-3.93840438103015,3.08041733073337));
#37964=CARTESIAN_POINT('',(3.95,-3.93840438103015,3.08041733073337));
#37965=CARTESIAN_POINT('',(7.4,-3.47521783996191,3.59483809994421));
#37966=CARTESIAN_POINT('Origin',(7.4,0.,0.));
#37967=CARTESIAN_POINT('',(0.6,-3.47521783996191,3.59483809994421));
#37968=CARTESIAN_POINT('',(3.95,-3.47521783996191,3.59483809994421));
#37969=CARTESIAN_POINT('',(0.6,-3.21188602036704,3.83194313529973));
#37970=CARTESIAN_POINT('Origin',(0.6,0.,0.));
#37971=CARTESIAN_POINT('',(7.4,-3.21188602036704,3.83194313529973));
#37972=CARTESIAN_POINT('',(3.95,-3.21188602036704,3.83194313529973));
#37973=CARTESIAN_POINT('',(7.4,-2.65186712461055,4.23882067955342));
#37974=CARTESIAN_POINT('Origin',(7.4,0.,0.));
#37975=CARTESIAN_POINT('',(0.6,-2.65186712461055,4.23882067955342));
#37976=CARTESIAN_POINT('',(3.95,-2.65186712461055,4.23882067955342));
#37977=CARTESIAN_POINT('',(0.6,-2.3449928282748,4.41599463715025));
#37978=CARTESIAN_POINT('Origin',(0.6,0.,0.));
#37979=CARTESIAN_POINT('',(7.4,-2.3449928282748,4.41599463715025));
#37980=CARTESIAN_POINT('',(3.95,-2.3449928282748,4.41599463715025));
#37981=CARTESIAN_POINT('',(7.4,-1.71261709084343,4.69754645534783));
#37982=CARTESIAN_POINT('Origin',(7.4,0.,0.));
#37983=CARTESIAN_POINT('',(0.6,-1.71261709084343,4.69754645534783));
#37984=CARTESIAN_POINT('',(3.95,-1.71261709084343,4.69754645534783));
#37985=CARTESIAN_POINT('',(0.6,-1.37561219706291,4.807045983064));
#37986=CARTESIAN_POINT('Origin',(0.6,0.,0.));
#37987=CARTESIAN_POINT('',(7.4,-1.37561219706291,4.807045983064));
#37988=CARTESIAN_POINT('',(3.95,-1.37561219706291,4.807045983064));
#37989=CARTESIAN_POINT('',(7.4,-0.698517472157877,4.95096690971473));
#37990=CARTESIAN_POINT('Origin',(7.4,0.,0.));
#37991=CARTESIAN_POINT('',(0.6,-0.698517472157877,4.95096690971473));
#37992=CARTESIAN_POINT('',(3.95,-0.698517472157877,4.95096690971473));
#37993=CARTESIAN_POINT('',(0.6,-0.346110711919694,4.98800635275201));
#37994=CARTESIAN_POINT('Origin',(0.6,0.,0.));
#37995=CARTESIAN_POINT('',(7.4,-0.346110711919694,4.98800635275201));
#37996=CARTESIAN_POINT('',(3.95,-0.346110711919694,4.98800635275201));
#37997=CARTESIAN_POINT('',(7.4,0.346110711919697,4.98800635275201));
#37998=CARTESIAN_POINT('Origin',(7.4,0.,0.));
#37999=CARTESIAN_POINT('',(0.6,0.346110711919695,4.98800635275201));
#38000=CARTESIAN_POINT('',(3.95,0.346110711919697,4.98800635275201));
#38001=CARTESIAN_POINT('',(0.6,0.698517472157879,4.95096690971472));
#38002=CARTESIAN_POINT('Origin',(0.6,0.,0.));
#38003=CARTESIAN_POINT('',(7.4,0.698517472157878,4.95096690971472));
#38004=CARTESIAN_POINT('',(3.95,0.698517472157878,4.95096690971472));
#38005=CARTESIAN_POINT('',(7.4,1.37561219706292,4.807045983064));
#38006=CARTESIAN_POINT('Origin',(7.4,0.,0.));
#38007=CARTESIAN_POINT('',(0.6,1.37561219706292,4.807045983064));
#38008=CARTESIAN_POINT('',(3.95,1.37561219706292,4.807045983064));
#38009=CARTESIAN_POINT('',(0.6,1.71261709084344,4.69754645534783));
#38010=CARTESIAN_POINT('Origin',(0.6,0.,0.));
#38011=CARTESIAN_POINT('',(7.4,1.71261709084344,4.69754645534783));
#38012=CARTESIAN_POINT('',(3.95,1.71261709084344,4.69754645534783));
#38013=CARTESIAN_POINT('',(7.4,2.3449928282748,4.41599463715025));
#38014=CARTESIAN_POINT('Origin',(7.4,0.,0.));
#38015=CARTESIAN_POINT('',(0.6,2.3449928282748,4.41599463715025));
#38016=CARTESIAN_POINT('',(3.95,2.3449928282748,4.41599463715025));
#38017=CARTESIAN_POINT('',(0.6,2.65186712461056,4.23882067955342));
#38018=CARTESIAN_POINT('Origin',(0.6,0.,0.));
#38019=CARTESIAN_POINT('',(7.4,2.65186712461056,4.23882067955342));
#38020=CARTESIAN_POINT('',(3.95,2.65186712461056,4.23882067955342));
#38021=CARTESIAN_POINT('',(7.4,3.21188602036705,3.83194313529973));
#38022=CARTESIAN_POINT('Origin',(7.4,0.,0.));
#38023=CARTESIAN_POINT('',(0.6,3.21188602036705,3.83194313529973));
#38024=CARTESIAN_POINT('',(3.95,3.21188602036705,3.83194313529973));
#38025=CARTESIAN_POINT('',(0.6,3.47521783996191,3.59483809994421));
#38026=CARTESIAN_POINT('Origin',(0.6,0.,0.));
#38027=CARTESIAN_POINT('',(7.4,3.47521783996191,3.59483809994421));
#38028=CARTESIAN_POINT('',(3.95,3.47521783996191,3.59483809994421));
#38029=CARTESIAN_POINT('',(7.4,3.93840438103015,3.08041733073337));
#38030=CARTESIAN_POINT('Origin',(7.4,0.,0.));
#38031=CARTESIAN_POINT('',(0.6,3.93840438103015,3.08041733073337));
#38032=CARTESIAN_POINT('',(3.95,3.93840438103015,3.08041733073337));
#38033=CARTESIAN_POINT('',(0.6,4.14668485976156,2.79374384542038));
#38034=CARTESIAN_POINT('Origin',(0.6,0.,0.));
#38035=CARTESIAN_POINT('',(7.4,4.14668485976156,2.79374384542038));
#38036=CARTESIAN_POINT('',(3.95,4.14668485976156,2.79374384542038));
#38037=CARTESIAN_POINT('',(7.4,4.49279557168126,2.19426250733163));
#38038=CARTESIAN_POINT('Origin',(7.4,0.,0.));
#38039=CARTESIAN_POINT('',(0.6,4.49279557168126,2.19426250733163));
#38040=CARTESIAN_POINT('',(3.95,4.49279557168126,2.19426250733163));
#38041=CARTESIAN_POINT('',(0.6,4.63692185318803,1.87054957898135));
#38042=CARTESIAN_POINT('Origin',(0.6,0.,0.));
#38043=CARTESIAN_POINT('',(7.4,4.63692185318803,1.87054957898135));
#38044=CARTESIAN_POINT('',(3.95,4.63692185318803,1.87054957898135));
#38045=CARTESIAN_POINT('',(7.4,4.85083003702482,1.21220788311979));
#38046=CARTESIAN_POINT('Origin',(7.4,0.,0.));
#38047=CARTESIAN_POINT('',(0.6,4.85083003702482,1.21220788311979));
#38048=CARTESIAN_POINT('',(3.95,4.85083003702482,1.21220788311979));
#38049=CARTESIAN_POINT('',(0.6,4.92450311121048,0.865603320048098));
#38050=CARTESIAN_POINT('Origin',(0.6,0.,0.));
#38051=CARTESIAN_POINT('',(7.4,4.92450311121048,0.865603320048098));
#38052=CARTESIAN_POINT('',(3.95,4.92450311121048,0.865603320048098));
#38053=CARTESIAN_POINT('',(7.4,4.99685995288536,0.177173957596825));
#38054=CARTESIAN_POINT('Origin',(7.4,0.,0.));
#38055=CARTESIAN_POINT('',(0.6,4.99685995288536,0.177173957596825));
#38056=CARTESIAN_POINT('',(3.95,4.99685995288536,0.177173957596825));
#38057=CARTESIAN_POINT('',(0.6,4.99685995288536,-0.177173957596824));
#38058=CARTESIAN_POINT('Origin',(0.6,0.,0.));
#38059=CARTESIAN_POINT('',(7.4,4.99685995288536,-0.177173957596824));
#38060=CARTESIAN_POINT('',(3.95,4.99685995288536,-0.177173957596824));
#38061=CARTESIAN_POINT('Origin',(7.4,0.,0.));
#38062=CARTESIAN_POINT('Origin',(0.6,4.70492030578719,-1.84847231956321));
#38063=CARTESIAN_POINT('',(7.6,4.38501819668448,-1.95233588676384));
#38064=CARTESIAN_POINT('Ctrl Pts',(7.6,4.38501819668448,-1.95233588676384));
#38065=CARTESIAN_POINT('Ctrl Pts',(7.5035787985868,4.50839957946168,-1.91227728703366));
#38066=CARTESIAN_POINT('Ctrl Pts',(7.4,4.63692185318803,-1.87054957898135));
#38067=CARTESIAN_POINT('',(0.6,4.38501819668448,-1.95233588676384));
#38068=CARTESIAN_POINT('',(0.6,4.38501819668448,-1.95233588676384));
#38069=CARTESIAN_POINT('',(0.6,4.70492030578719,-1.84847231956321));
#38070=CARTESIAN_POINT('Origin',(0.6,4.49921137888981,-2.00317796714832));
#38071=CARTESIAN_POINT('',(0.6,4.38501819668448,-1.95233588676384));
#38072=CARTESIAN_POINT('Origin',(0.6,4.38501819668448,-1.95233588676384));
#38073=CARTESIAN_POINT('Ctrl Pts',(7.4,4.49279557168125,-2.19426250733164));
#38074=CARTESIAN_POINT('Ctrl Pts',(7.50357879858675,4.43780711505025,-2.07083055806237));
#38075=CARTESIAN_POINT('Ctrl Pts',(7.6,4.38501819668448,-1.95233588676385));
#38076=CARTESIAN_POINT('Origin',(0.6,4.21778750335929,-2.78628670034263));
#38077=CARTESIAN_POINT('',(7.6,3.88328157299975,-2.82136921100387));
#38078=CARTESIAN_POINT('Ctrl Pts',(7.6,3.88328157299975,-2.82136921100387));
#38079=CARTESIAN_POINT('Ctrl Pts',(7.50357879858666,4.01229542774037,-2.80783841969766));
#38080=CARTESIAN_POINT('Ctrl Pts',(7.4,4.14668485976156,-2.79374384542038));
#38081=CARTESIAN_POINT('',(0.6,3.88328157299975,-2.82136921100387));
#38082=CARTESIAN_POINT('',(0.6,3.88328157299975,-2.82136921100387));
#38083=CARTESIAN_POINT('',(0.6,4.21778750335929,-2.78628670034263));
#38084=CARTESIAN_POINT('Origin',(0.6,3.98440869729662,-2.89484236754043));
#38085=CARTESIAN_POINT('',(0.6,3.88328157299975,-2.82136921100387));
#38086=CARTESIAN_POINT('Origin',(0.6,3.88328157299975,-2.82136921100387));
#38087=CARTESIAN_POINT('Ctrl Pts',(7.4,3.93840438103015,-3.08041733073338));
#38088=CARTESIAN_POINT('Ctrl Pts',(7.50357879858664,3.91028049938202,-2.94824992270828));
#38089=CARTESIAN_POINT('Ctrl Pts',(7.6,3.88328157299975,-2.82136921100387));
#38090=CARTESIAN_POINT('Origin',(0.6,3.54631714784465,-3.6023269822301));
#38091=CARTESIAN_POINT('',(7.6,3.21182691052252,-3.56709516229149));
#38092=CARTESIAN_POINT('Ctrl Pts',(7.6,3.21182691052252,-3.56709516229149));
#38093=CARTESIAN_POINT('Ctrl Pts',(7.50357879858679,3.34083471269687,-3.58068353991731));
#38094=CARTESIAN_POINT('Ctrl Pts',(7.4,3.47521783996191,-3.59483809994421));
#38095=CARTESIAN_POINT('',(0.6,3.21182691052252,-3.56709516229149));
#38096=CARTESIAN_POINT('',(0.6,3.21182691052252,-3.56709516229149));
#38097=CARTESIAN_POINT('',(0.6,3.54631714784465,-3.6023269822301));
#38098=CARTESIAN_POINT('Origin',(0.6,3.29546823631738,-3.65998826547617));
#38099=CARTESIAN_POINT('',(0.6,3.21182691052252,-3.56709516229149));
#38100=CARTESIAN_POINT('Origin',(0.6,3.21182691052252,-3.56709516229149));
#38101=CARTESIAN_POINT('Ctrl Pts',(7.4,3.21188602036704,-3.83194313529974));
#38102=CARTESIAN_POINT('Ctrl Pts',(7.50357879858676,3.2118558622831,-3.6968166184588));
#38103=CARTESIAN_POINT('Ctrl Pts',(7.6,3.21182691052252,-3.56709516229149));
#38104=CARTESIAN_POINT('Origin',(0.6,2.71985571585149,-4.26092828911142));
#38105=CARTESIAN_POINT('',(7.6,2.4,-4.15692193816531));
#38106=CARTESIAN_POINT('Ctrl Pts',(7.6,2.4,-4.15692193816531));
#38107=CARTESIAN_POINT('Ctrl Pts',(7.5035787985868,2.52336348960512,-4.19703560741661));
#38108=CARTESIAN_POINT('Ctrl Pts',(7.4,2.65186712461055,-4.23882067955342));
#38109=CARTESIAN_POINT('',(0.6,2.4,-4.15692193816531));
#38110=CARTESIAN_POINT('',(0.6,2.4,-4.15692193816531));
#38111=CARTESIAN_POINT('',(0.6,2.71985571585149,-4.26092828911142));
#38112=CARTESIAN_POINT('Origin',(0.6,2.4625,-4.26517511363836));
#38113=CARTESIAN_POINT('',(0.6,2.4,-4.15692193816531));
#38114=CARTESIAN_POINT('Origin',(0.6,2.4,-4.15692193816531));
#38115=CARTESIAN_POINT('Ctrl Pts',(7.4,2.3449928282748,-4.41599463715025));
#38116=CARTESIAN_POINT('Ctrl Pts',(7.50357879858669,2.37305771180804,-4.28381468868864));
#38117=CARTESIAN_POINT('Ctrl Pts',(7.6,2.4,-4.15692193816531));
#38118=CARTESIAN_POINT('Origin',(0.6,1.77452353775989,-4.73330658355616));
#38119=CARTESIAN_POINT('',(7.6,1.48328157299975,-4.56507127821674));
#38120=CARTESIAN_POINT('Ctrl Pts',(7.6,1.48328157299975,-4.56507127821674));
#38121=CARTESIAN_POINT('Ctrl Pts',(7.50357879858666,1.59560917357637,-4.62995707926061));
#38122=CARTESIAN_POINT('Ctrl Pts',(7.4,1.71261709084344,-4.69754645534783));
#38123=CARTESIAN_POINT('',(0.6,1.48328157299975,-4.56507127821674));
#38124=CARTESIAN_POINT('',(0.6,1.48328157299975,-4.56507127821674));
#38125=CARTESIAN_POINT('',(0.6,1.77452353775989,-4.73330658355616));
#38126=CARTESIAN_POINT('Origin',(0.6,1.52190869729661,-4.68395334275363));
#38127=CARTESIAN_POINT('',(0.6,1.48328157299975,-4.56507127821674));
#38128=CARTESIAN_POINT('Origin',(0.6,1.48328157299975,-4.56507127821674));
#38129=CARTESIAN_POINT('Ctrl Pts',(7.4,1.37561219706291,-4.807045983064));
#38130=CARTESIAN_POINT('Ctrl Pts',(7.50357879858666,1.43054555213267,-4.68358950099919));
#38131=CARTESIAN_POINT('Ctrl Pts',(7.6,1.48328157299975,-4.56507127821674));
#38132=CARTESIAN_POINT('Origin',(0.6,0.751636165959509,-4.99881666737456));
#38133=CARTESIAN_POINT('',(7.6,0.501736623684734,-4.77370509776771));
#38134=CARTESIAN_POINT('Ctrl Pts',(7.6,0.501736623684735,-4.77370509776771));
#38135=CARTESIAN_POINT('Ctrl Pts',(7.50357879858666,0.59811908007984,-4.86052720974185));
#38136=CARTESIAN_POINT('Ctrl Pts',(7.4,0.698517472157876,-4.95096690971473));
#38137=CARTESIAN_POINT('',(0.6,0.501736623684734,-4.77370509776771));
#38138=CARTESIAN_POINT('',(0.6,0.501736623684734,-4.77370509776771));
#38139=CARTESIAN_POINT('',(0.6,0.751636165959509,-4.99881666737456));
#38140=CARTESIAN_POINT('Origin',(0.6,0.514802681593191,-4.89802033468875));
#38141=CARTESIAN_POINT('',(0.6,0.501736623684734,-4.77370509776771));
#38142=CARTESIAN_POINT('Origin',(0.6,0.501736623684734,-4.77370509776771));
#38143=CARTESIAN_POINT('Ctrl Pts',(7.4,0.346110711919692,-4.98800635275201));
#38144=CARTESIAN_POINT('Ctrl Pts',(7.50357879858676,0.425511687310016,-4.87866897776003));
#38145=CARTESIAN_POINT('Ctrl Pts',(7.6,0.501736623684734,-4.77370509776771));
#38146=CARTESIAN_POINT('Origin',(0.6,-0.304101313043792,-5.045854475845));
#38147=CARTESIAN_POINT('',(7.6,-0.50173662368474,-4.77370509776771));
#38148=CARTESIAN_POINT('Ctrl Pts',(7.6,-0.50173662368474,-4.77370509776771));
#38149=CARTESIAN_POINT('Ctrl Pts',(7.50357879858676,-0.425511687310022,
-4.87866897776003));
#38150=CARTESIAN_POINT('Ctrl Pts',(7.4,-0.346110711919699,-4.98800635275201));
#38151=CARTESIAN_POINT('',(0.6,-0.50173662368474,-4.77370509776771));
#38152=CARTESIAN_POINT('',(0.6,-0.50173662368474,-4.77370509776771));
#38153=CARTESIAN_POINT('',(0.6,-0.304101313043792,-5.045854475845));
#38154=CARTESIAN_POINT('Origin',(0.6,-0.514802681593197,-4.89802033468875));
#38155=CARTESIAN_POINT('',(0.6,-0.50173662368474,-4.77370509776771));
#38156=CARTESIAN_POINT('Origin',(0.6,-0.50173662368474,-4.77370509776771));
#38157=CARTESIAN_POINT('Ctrl Pts',(7.4,-0.698517472157881,-4.95096690971472));
#38158=CARTESIAN_POINT('Ctrl Pts',(7.50357879858675,-0.598119080079759,
-4.86052720974177));
#38159=CARTESIAN_POINT('Ctrl Pts',(7.6,-0.501736623684741,-4.77370509776771));
#38160=CARTESIAN_POINT('Origin',(0.6,-1.34654810542708,-4.87236423102489));
#38161=CARTESIAN_POINT('',(7.6,-1.48328157299975,-4.56507127821674));
#38162=CARTESIAN_POINT('Ctrl Pts',(7.6,-1.48328157299975,-4.56507127821674));
#38163=CARTESIAN_POINT('Ctrl Pts',(7.50357879858675,-1.43054555213272,-4.68358950099908));
#38164=CARTESIAN_POINT('Ctrl Pts',(7.4,-1.37561219706292,-4.807045983064));
#38165=CARTESIAN_POINT('',(0.6,-1.48328157299975,-4.56507127821674));
#38166=CARTESIAN_POINT('',(0.6,-1.48328157299975,-4.56507127821674));
#38167=CARTESIAN_POINT('',(0.6,-1.34654810542708,-4.87236423102489));
#38168=CARTESIAN_POINT('Origin',(0.6,-1.52190869729662,-4.68395334275363));
#38169=CARTESIAN_POINT('',(0.6,-1.48328157299975,-4.56507127821674));
#38170=CARTESIAN_POINT('Origin',(0.6,-1.48328157299975,-4.56507127821674));
#38171=CARTESIAN_POINT('Ctrl Pts',(7.4,-1.71261709084344,-4.69754645534783));
#38172=CARTESIAN_POINT('Ctrl Pts',(7.50357879858678,-1.59560917357623,-4.62995707926053));
#38173=CARTESIAN_POINT('Ctrl Pts',(7.6,-1.48328157299975,-4.56507127821674));
#38174=CARTESIAN_POINT('Origin',(0.6,-2.3301442841485,-4.48592828911141));
#38175=CARTESIAN_POINT('',(7.6,-2.4,-4.1569219381653));
#38176=CARTESIAN_POINT('Ctrl Pts',(7.6,-2.4,-4.15692193816531));
#38177=CARTESIAN_POINT('Ctrl Pts',(7.50357879858655,-2.37305771180801,-4.28381468868881));
#38178=CARTESIAN_POINT('Ctrl Pts',(7.4,-2.34499282827481,-4.41599463715025));
#38179=CARTESIAN_POINT('',(0.6,-2.4,-4.1569219381653));
#38180=CARTESIAN_POINT('',(0.6,-2.4,-4.1569219381653));
#38181=CARTESIAN_POINT('',(0.6,-2.3301442841485,-4.48592828911141));
#38182=CARTESIAN_POINT('Origin',(0.6,-2.4625,-4.26517511363836));
#38183=CARTESIAN_POINT('',(0.6,-2.4,-4.1569219381653));
#38184=CARTESIAN_POINT('Origin',(0.6,-2.4,-4.1569219381653));
#38185=CARTESIAN_POINT('Ctrl Pts',(7.4,-2.65186712461056,-4.23882067955342));
#38186=CARTESIAN_POINT('Ctrl Pts',(7.5035787985868,-2.52336348960513,-4.19703560741661));
#38187=CARTESIAN_POINT('Ctrl Pts',(7.6,-2.4,-4.1569219381653));
#38188=CARTESIAN_POINT('Origin',(0.6,-3.21190197637982,-3.90343575509158));
#38189=CARTESIAN_POINT('',(7.6,-3.21182691052252,-3.56709516229149));
#38190=CARTESIAN_POINT('Ctrl Pts',(7.6,-3.21182691052252,-3.56709516229149));
#38191=CARTESIAN_POINT('Ctrl Pts',(7.5035787985866,-3.2118558622831,-3.69681661845901));
#38192=CARTESIAN_POINT('Ctrl Pts',(7.4,-3.21188602036705,-3.83194313529973));
#38193=CARTESIAN_POINT('',(0.6,-3.21182691052252,-3.56709516229149));
#38194=CARTESIAN_POINT('',(0.6,-3.21182691052252,-3.56709516229149));
#38195=CARTESIAN_POINT('',(0.6,-3.21190197637982,-3.90343575509158));
#38196=CARTESIAN_POINT('Origin',(0.6,-3.29546823631738,-3.65998826547617));
#38197=CARTESIAN_POINT('',(0.6,-3.21182691052252,-3.56709516229149));
#38198=CARTESIAN_POINT('Origin',(0.6,-3.21182691052252,-3.56709516229149));
#38199=CARTESIAN_POINT('Ctrl Pts',(7.4,-3.47521783996191,-3.59483809994421));
#38200=CARTESIAN_POINT('Ctrl Pts',(7.5035787985868,-3.34083471269686,-3.58068353991731));
#38201=CARTESIAN_POINT('Ctrl Pts',(7.6,-3.21182691052252,-3.56709516229149));
#38202=CARTESIAN_POINT('Origin',(0.6,-3.95328413982768,-3.15034434781135));
#38203=CARTESIAN_POINT('',(7.6,-3.88328157299975,-2.82136921100387));
#38204=CARTESIAN_POINT('Ctrl Pts',(7.6,-3.88328157299975,-2.82136921100387));
#38205=CARTESIAN_POINT('Ctrl Pts',(7.50357879858668,-3.91028049938201,-2.94824992270822));
#38206=CARTESIAN_POINT('Ctrl Pts',(7.4,-3.93840438103015,-3.08041733073337));
#38207=CARTESIAN_POINT('',(0.6,-3.88328157299975,-2.82136921100387));
#38208=CARTESIAN_POINT('',(0.6,-3.88328157299975,-2.82136921100387));
#38209=CARTESIAN_POINT('',(0.6,-3.95328413982768,-3.15034434781135));
#38210=CARTESIAN_POINT('Origin',(0.6,-3.98440869729662,-2.89484236754043));
#38211=CARTESIAN_POINT('',(0.6,-3.88328157299975,-2.82136921100387));
#38212=CARTESIAN_POINT('Origin',(0.6,-3.88328157299975,-2.82136921100387));
#38213=CARTESIAN_POINT('Ctrl Pts',(7.4,-4.14668485976156,-2.79374384542038));
#38214=CARTESIAN_POINT('Ctrl Pts',(7.50357879858676,-4.01229542774023,-2.80783841969767));
#38215=CARTESIAN_POINT('Ctrl Pts',(7.6,-3.88328157299975,-2.82136921100387));
#38216=CARTESIAN_POINT('Origin',(0.6,-4.52188881640308,-2.25956777550237));
#38217=CARTESIAN_POINT('',(7.6,-4.38501819668449,-1.95233588676384));
#38218=CARTESIAN_POINT('Ctrl Pts',(7.6,-4.38501819668449,-1.95233588676384));
#38219=CARTESIAN_POINT('Ctrl Pts',(7.50357879858659,-4.43780711505034,-2.07083055806256));
#38220=CARTESIAN_POINT('Ctrl Pts',(7.4,-4.49279557168126,-2.19426250733163));
#38221=CARTESIAN_POINT('',(0.6,-4.38501819668449,-1.95233588676384));
#38222=CARTESIAN_POINT('',(0.6,-4.38501819668449,-1.95233588676384));
#38223=CARTESIAN_POINT('',(0.6,-4.52188881640308,-2.25956777550237));
#38224=CARTESIAN_POINT('Origin',(0.6,-4.49921137888981,-2.00317796714831));
#38225=CARTESIAN_POINT('',(0.6,-4.38501819668449,-1.95233588676384));
#38226=CARTESIAN_POINT('Origin',(0.6,-4.38501819668449,-1.95233588676384));
#38227=CARTESIAN_POINT('Ctrl Pts',(7.4,-4.63692185318803,-1.87054957898135));
#38228=CARTESIAN_POINT('Ctrl Pts',(7.50357879858679,-4.5083995794617,-1.91227728703365));
#38229=CARTESIAN_POINT('Ctrl Pts',(7.6,-4.38501819668449,-1.95233588676384));
#38230=CARTESIAN_POINT('Origin',(0.6,-4.89286525327172,-1.27003724879479));
#38231=CARTESIAN_POINT('',(7.6,-4.69510848352227,-0.997976115925243));
#38232=CARTESIAN_POINT('Ctrl Pts',(7.6,-4.69510848352227,-0.997976115925244));
#38233=CARTESIAN_POINT('Ctrl Pts',(7.50357879858667,-4.77138026482971,-1.10290596108185));
#38234=CARTESIAN_POINT('Ctrl Pts',(7.4,-4.85083003702482,-1.21220788311979));
#38235=CARTESIAN_POINT('',(0.6,-4.69510848352227,-0.997976115925243));
#38236=CARTESIAN_POINT('',(0.6,-4.69510848352227,-0.997976115925243));
#38237=CARTESIAN_POINT('',(0.6,-4.89286525327172,-1.27003724879479));
#38238=CARTESIAN_POINT('Origin',(0.6,-4.81737693361399,-1.02396507727746));
#38239=CARTESIAN_POINT('',(0.6,-4.69510848352227,-0.997976115925243));
#38240=CARTESIAN_POINT('Origin',(0.6,-4.69510848352227,-0.997976115925243));
#38241=CARTESIAN_POINT('Ctrl Pts',(7.4,-4.92450311121048,-0.865603320048097));
#38242=CARTESIAN_POINT('Ctrl Pts',(7.50357879858677,-4.80746503585935,-0.933140460801746));
#38243=CARTESIAN_POINT('Ctrl Pts',(7.6,-4.69510848352227,-0.997976115925243));
#38244=CARTESIAN_POINT('Origin',(0.6,-5.05,-0.224999999999999));
#38245=CARTESIAN_POINT('',(7.6,-4.8,5.87830463590729E-16));
#38246=CARTESIAN_POINT('Ctrl Pts',(7.6,-4.8,-2.83461197776636E-16));
#38247=CARTESIAN_POINT('Ctrl Pts',(7.50357879858684,-4.89642120141316,-0.0867790812718465));
#38248=CARTESIAN_POINT('Ctrl Pts',(7.4,-4.99685995288536,-0.177173957596824));
#38249=CARTESIAN_POINT('',(0.6,-4.8,5.87830463590729E-16));
#38250=CARTESIAN_POINT('',(0.6,-4.8,5.87830463590729E-16));
#38251=CARTESIAN_POINT('',(0.6,-5.05,-0.224999999999999));
#38252=CARTESIAN_POINT('Origin',(0.6,-4.925,6.03138548580071E-16));
#38253=CARTESIAN_POINT('',(0.6,-4.8,5.87830463590729E-16));
#38254=CARTESIAN_POINT('Origin',(0.6,-4.8,5.87830463590729E-16));
#38255=CARTESIAN_POINT('Ctrl Pts',(7.4,-4.99685995288536,0.177173957596825));
#38256=CARTESIAN_POINT('Ctrl Pts',(7.50357879858667,-4.89642120141333,0.0867790812719992));
#38257=CARTESIAN_POINT('Ctrl Pts',(7.6,-4.8,1.41730598888318E-15));
#38258=CARTESIAN_POINT('Origin',(0.6,-4.98642551413971,0.82987082846458));
#38259=CARTESIAN_POINT('',(7.6,-4.69510848352227,0.997976115925247));
#38260=CARTESIAN_POINT('Ctrl Pts',(7.6,-4.69510848352227,0.997976115925246));
#38261=CARTESIAN_POINT('Ctrl Pts',(7.50357879858674,-4.80746503585938,0.933140460801728));
#38262=CARTESIAN_POINT('Ctrl Pts',(7.4,-4.92450311121048,0.8656033200481));
#38263=CARTESIAN_POINT('',(0.6,-4.69510848352227,0.997976115925247));
#38264=CARTESIAN_POINT('',(0.6,-4.69510848352227,0.997976115925247));
#38265=CARTESIAN_POINT('',(0.6,-4.98642551413971,0.82987082846458));
#38266=CARTESIAN_POINT('Origin',(0.6,-4.81737693361399,1.02396507727747));
#38267=CARTESIAN_POINT('',(0.6,-4.69510848352227,0.997976115925247));
#38268=CARTESIAN_POINT('Origin',(0.6,-4.69510848352227,0.997976115925247));
#38269=CARTESIAN_POINT('Ctrl Pts',(7.4,-4.85083003702482,1.21220788311979));
#38270=CARTESIAN_POINT('Ctrl Pts',(7.50357879858672,-4.77138026482967,1.1029059610818));
#38271=CARTESIAN_POINT('Ctrl Pts',(7.6,-4.69510848352227,0.997976115925247));
#38272=CARTESIAN_POINT('Origin',(0.6,-4.70492030578719,1.84847231956321));
#38273=CARTESIAN_POINT('',(7.6,-4.38501819668448,1.95233588676384));
#38274=CARTESIAN_POINT('Ctrl Pts',(7.6,-4.38501819668448,1.95233588676384));
#38275=CARTESIAN_POINT('Ctrl Pts',(7.50357879858671,-4.50839957946179,1.91227728703362));
#38276=CARTESIAN_POINT('Ctrl Pts',(7.4,-4.63692185318803,1.87054957898135));
#38277=CARTESIAN_POINT('',(0.6,-4.38501819668448,1.95233588676384));
#38278=CARTESIAN_POINT('',(0.6,-4.38501819668448,1.95233588676384));
#38279=CARTESIAN_POINT('',(0.6,-4.70492030578719,1.84847231956321));
#38280=CARTESIAN_POINT('Origin',(0.6,-4.49921137888981,2.00317796714832));
#38281=CARTESIAN_POINT('',(0.6,-4.38501819668448,1.95233588676384));
#38282=CARTESIAN_POINT('Origin',(0.6,-4.38501819668448,1.95233588676384));
#38283=CARTESIAN_POINT('Ctrl Pts',(7.4,-4.49279557168125,2.19426250733164));
#38284=CARTESIAN_POINT('Ctrl Pts',(7.50357879858679,-4.43780711505023,2.07083055806232));
#38285=CARTESIAN_POINT('Ctrl Pts',(7.6,-4.38501819668448,1.95233588676384));
#38286=CARTESIAN_POINT('Origin',(0.6,-4.21778750335929,2.78628670034263));
#38287=CARTESIAN_POINT('',(7.6,-3.88328157299975,2.82136921100387));
#38288=CARTESIAN_POINT('Ctrl Pts',(7.6,-3.88328157299975,2.82136921100387));
#38289=CARTESIAN_POINT('Ctrl Pts',(7.50357879858675,-4.01229542774025,2.80783841969767));
#38290=CARTESIAN_POINT('Ctrl Pts',(7.4,-4.14668485976156,2.79374384542038));
#38291=CARTESIAN_POINT('',(0.6,-3.88328157299975,2.82136921100387));
#38292=CARTESIAN_POINT('',(0.6,-3.88328157299975,2.82136921100387));
#38293=CARTESIAN_POINT('',(0.6,-4.21778750335929,2.78628670034263));
#38294=CARTESIAN_POINT('Origin',(0.6,-3.98440869729662,2.89484236754043));
#38295=CARTESIAN_POINT('',(0.6,-3.88328157299975,2.82136921100387));
#38296=CARTESIAN_POINT('Origin',(0.6,-3.88328157299975,2.82136921100387));
#38297=CARTESIAN_POINT('Ctrl Pts',(7.4,-3.93840438103015,3.08041733073337));
#38298=CARTESIAN_POINT('Ctrl Pts',(7.50357879858669,-3.910280499382,2.94824992270821));
#38299=CARTESIAN_POINT('Ctrl Pts',(7.6,-3.88328157299975,2.82136921100387));
#38300=CARTESIAN_POINT('Origin',(0.6,-3.54631714784465,3.6023269822301));
#38301=CARTESIAN_POINT('',(7.6,-3.21182691052252,3.56709516229149));
#38302=CARTESIAN_POINT('Ctrl Pts',(7.6,-3.21182691052252,3.56709516229149));
#38303=CARTESIAN_POINT('Ctrl Pts',(7.50357879858679,-3.34083471269687,3.58068353991731));
#38304=CARTESIAN_POINT('Ctrl Pts',(7.4,-3.47521783996191,3.59483809994421));
#38305=CARTESIAN_POINT('',(0.6,-3.21182691052252,3.56709516229149));
#38306=CARTESIAN_POINT('',(0.6,-3.21182691052252,3.56709516229149));
#38307=CARTESIAN_POINT('',(0.6,-3.54631714784465,3.6023269822301));
#38308=CARTESIAN_POINT('Origin',(0.6,-3.29546823631738,3.65998826547617));
#38309=CARTESIAN_POINT('',(0.6,-3.21182691052252,3.56709516229149));
#38310=CARTESIAN_POINT('Origin',(0.6,-3.21182691052252,3.56709516229149));
#38311=CARTESIAN_POINT('Ctrl Pts',(7.4,-3.21188602036704,3.83194313529973));
#38312=CARTESIAN_POINT('Ctrl Pts',(7.50357879858653,-3.2118558622831,3.69681661845911));
#38313=CARTESIAN_POINT('Ctrl Pts',(7.6,-3.21182691052252,3.5670951622915));
#38314=CARTESIAN_POINT('Origin',(0.6,-2.7198557158515,4.26092828911142));
#38315=CARTESIAN_POINT('',(7.6,-2.4,4.15692193816531));
#38316=CARTESIAN_POINT('Ctrl Pts',(7.6,-2.4,4.15692193816531));
#38317=CARTESIAN_POINT('Ctrl Pts',(7.50357879858686,-2.52336348960505,4.19703560741659));
#38318=CARTESIAN_POINT('Ctrl Pts',(7.4,-2.65186712461055,4.23882067955342));
#38319=CARTESIAN_POINT('',(0.6,-2.4,4.15692193816531));
#38320=CARTESIAN_POINT('',(0.6,-2.4,4.15692193816531));
#38321=CARTESIAN_POINT('',(0.6,-2.7198557158515,4.26092828911142));
#38322=CARTESIAN_POINT('Origin',(0.6,-2.4625,4.26517511363836));
#38323=CARTESIAN_POINT('',(0.6,-2.4,4.15692193816531));
#38324=CARTESIAN_POINT('Origin',(0.6,-2.4,4.15692193816531));
#38325=CARTESIAN_POINT('Ctrl Pts',(7.4,-2.3449928282748,4.41599463715025));
#38326=CARTESIAN_POINT('Ctrl Pts',(7.50357879858658,-2.37305771180802,4.28381468868878));
#38327=CARTESIAN_POINT('Ctrl Pts',(7.6,-2.4,4.15692193816531));
#38328=CARTESIAN_POINT('Origin',(0.6,-1.77452353775989,4.73330658355616));
#38329=CARTESIAN_POINT('',(7.6,-1.48328157299975,4.56507127821674));
#38330=CARTESIAN_POINT('Ctrl Pts',(7.6,-1.48328157299975,4.56507127821674));
#38331=CARTESIAN_POINT('Ctrl Pts',(7.50357879858684,-1.59560917357616,4.62995707926049));
#38332=CARTESIAN_POINT('Ctrl Pts',(7.4,-1.71261709084344,4.69754645534783));
#38333=CARTESIAN_POINT('',(0.6,-1.48328157299975,4.56507127821674));
#38334=CARTESIAN_POINT('',(0.6,-1.48328157299975,4.56507127821674));
#38335=CARTESIAN_POINT('',(0.6,-1.77452353775989,4.73330658355616));
#38336=CARTESIAN_POINT('Origin',(0.6,-1.52190869729662,4.68395334275363));
#38337=CARTESIAN_POINT('',(0.6,-1.48328157299975,4.56507127821674));
#38338=CARTESIAN_POINT('Origin',(0.6,-1.48328157299975,4.56507127821674));
#38339=CARTESIAN_POINT('Ctrl Pts',(7.4,-1.37561219706291,4.807045983064));
#38340=CARTESIAN_POINT('Ctrl Pts',(7.50357879858665,-1.43054555213267,4.6835895009992));
#38341=CARTESIAN_POINT('Ctrl Pts',(7.6,-1.48328157299975,4.56507127821674));
#38342=CARTESIAN_POINT('Origin',(0.6,-0.751636165959511,4.99881666737456));
#38343=CARTESIAN_POINT('',(7.6,-0.501736623684736,4.77370509776771));
#38344=CARTESIAN_POINT('Ctrl Pts',(7.6,-0.501736623684736,4.77370509776771));
#38345=CARTESIAN_POINT('Ctrl Pts',(7.5035787985868,-0.598119080079706,4.86052720974173));
#38346=CARTESIAN_POINT('Ctrl Pts',(7.4,-0.698517472157876,4.95096690971472));
#38347=CARTESIAN_POINT('',(0.6,-0.501736623684736,4.77370509776771));
#38348=CARTESIAN_POINT('',(0.6,-0.501736623684736,4.77370509776771));
#38349=CARTESIAN_POINT('',(0.6,-0.751636165959511,4.99881666737456));
#38350=CARTESIAN_POINT('Origin',(0.6,-0.514802681593193,4.89802033468875));
#38351=CARTESIAN_POINT('',(0.6,-0.501736623684736,4.77370509776771));
#38352=CARTESIAN_POINT('Origin',(0.6,-0.501736623684736,4.77370509776771));
#38353=CARTESIAN_POINT('Ctrl Pts',(7.4,-0.346110711919695,4.98800635275201));
#38354=CARTESIAN_POINT('Ctrl Pts',(7.50357879858677,-0.425511687310028,
4.87866897776002));
#38355=CARTESIAN_POINT('Ctrl Pts',(7.6,-0.501736623684736,4.77370509776771));
#38356=CARTESIAN_POINT('Origin',(0.6,0.30410131304379,5.045854475845));
#38357=CARTESIAN_POINT('',(7.6,0.501736623684738,4.77370509776771));
#38358=CARTESIAN_POINT('Ctrl Pts',(7.6,0.501736623684738,4.77370509776771));
#38359=CARTESIAN_POINT('Ctrl Pts',(7.50357879858681,0.425511687310058,4.87866897775998));
#38360=CARTESIAN_POINT('Ctrl Pts',(7.4,0.346110711919696,4.98800635275201));
#38361=CARTESIAN_POINT('',(0.6,0.501736623684738,4.77370509776771));
#38362=CARTESIAN_POINT('',(0.6,0.501736623684738,4.77370509776771));
#38363=CARTESIAN_POINT('',(0.6,0.30410131304379,5.045854475845));
#38364=CARTESIAN_POINT('Origin',(0.6,0.514802681593194,4.89802033468875));
#38365=CARTESIAN_POINT('',(0.6,0.501736623684738,4.77370509776771));
#38366=CARTESIAN_POINT('Origin',(0.6,0.501736623684738,4.77370509776771));
#38367=CARTESIAN_POINT('Ctrl Pts',(7.4,0.698517472157879,4.95096690971472));
#38368=CARTESIAN_POINT('Ctrl Pts',(7.50357879858674,0.598119080079767,4.86052720974178));
#38369=CARTESIAN_POINT('Ctrl Pts',(7.6,0.501736623684738,4.77370509776771));
#38370=CARTESIAN_POINT('Origin',(0.6,1.34654810542708,4.87236423102489));
#38371=CARTESIAN_POINT('',(7.6,1.48328157299975,4.56507127821674));
#38372=CARTESIAN_POINT('Ctrl Pts',(7.6,1.48328157299975,4.56507127821674));
#38373=CARTESIAN_POINT('Ctrl Pts',(7.50357879858677,1.43054555213273,4.68358950099906));
#38374=CARTESIAN_POINT('Ctrl Pts',(7.4,1.37561219706292,4.807045983064));
#38375=CARTESIAN_POINT('',(0.6,1.48328157299975,4.56507127821674));
#38376=CARTESIAN_POINT('',(0.6,1.48328157299975,4.56507127821674));
#38377=CARTESIAN_POINT('',(0.6,1.34654810542708,4.87236423102489));
#38378=CARTESIAN_POINT('Origin',(0.6,1.52190869729662,4.68395334275363));
#38379=CARTESIAN_POINT('',(0.6,1.48328157299975,4.56507127821674));
#38380=CARTESIAN_POINT('Origin',(0.6,1.48328157299975,4.56507127821674));
#38381=CARTESIAN_POINT('Ctrl Pts',(7.4,1.71261709084344,4.69754645534783));
#38382=CARTESIAN_POINT('Ctrl Pts',(7.50357879858672,1.59560917357629,4.62995707926056));
#38383=CARTESIAN_POINT('Ctrl Pts',(7.6,1.48328157299975,4.56507127821674));
#38384=CARTESIAN_POINT('Origin',(0.6,2.3301442841485,4.48592828911142));
#38385=CARTESIAN_POINT('',(7.6,2.4,4.15692193816531));
#38386=CARTESIAN_POINT('Ctrl Pts',(7.6,2.4,4.15692193816531));
#38387=CARTESIAN_POINT('Ctrl Pts',(7.50357879858657,2.37305771180801,4.28381468868879));
#38388=CARTESIAN_POINT('Ctrl Pts',(7.4,2.3449928282748,4.41599463715025));
#38389=CARTESIAN_POINT('',(0.6,2.4,4.15692193816531));
#38390=CARTESIAN_POINT('',(0.6,2.4,4.15692193816531));
#38391=CARTESIAN_POINT('',(0.6,2.3301442841485,4.48592828911142));
#38392=CARTESIAN_POINT('Origin',(0.6,2.4625,4.26517511363836));
#38393=CARTESIAN_POINT('',(0.6,2.4,4.15692193816531));
#38394=CARTESIAN_POINT('Origin',(0.6,2.4,4.15692193816531));
#38395=CARTESIAN_POINT('Ctrl Pts',(7.4,2.65186712461056,4.23882067955342));
#38396=CARTESIAN_POINT('Ctrl Pts',(7.50357879858673,2.52336348960521,4.19703560741664));
#38397=CARTESIAN_POINT('Ctrl Pts',(7.6,2.4,4.15692193816531));
#38398=CARTESIAN_POINT('Origin',(0.6,3.21190197637982,3.90343575509158));
#38399=CARTESIAN_POINT('',(7.6,3.21182691052252,3.56709516229149));
#38400=CARTESIAN_POINT('Ctrl Pts',(7.6,3.21182691052252,3.56709516229149));
#38401=CARTESIAN_POINT('Ctrl Pts',(7.5035787985867,3.2118558622831,3.69681661845887));
#38402=CARTESIAN_POINT('Ctrl Pts',(7.4,3.21188602036705,3.83194313529973));
#38403=CARTESIAN_POINT('',(0.6,3.21182691052252,3.56709516229149));
#38404=CARTESIAN_POINT('',(0.6,3.21182691052252,3.56709516229149));
#38405=CARTESIAN_POINT('',(0.6,3.21190197637982,3.90343575509158));
#38406=CARTESIAN_POINT('Origin',(0.6,3.29546823631738,3.65998826547617));
#38407=CARTESIAN_POINT('',(0.6,3.21182691052252,3.56709516229149));
#38408=CARTESIAN_POINT('Origin',(0.6,3.21182691052252,3.56709516229149));
#38409=CARTESIAN_POINT('Ctrl Pts',(7.4,3.47521783996191,3.59483809994421));
#38410=CARTESIAN_POINT('Ctrl Pts',(7.50357879858682,3.34083471269684,3.58068353991731));
#38411=CARTESIAN_POINT('Ctrl Pts',(7.6,3.21182691052252,3.56709516229149));
#38412=CARTESIAN_POINT('Origin',(0.6,3.95328413982768,3.15034434781135));
#38413=CARTESIAN_POINT('',(7.6,3.88328157299975,2.82136921100387));
#38414=CARTESIAN_POINT('Ctrl Pts',(7.6,3.88328157299975,2.82136921100387));
#38415=CARTESIAN_POINT('Ctrl Pts',(7.50357879858661,3.91028049938203,2.94824992270832));
#38416=CARTESIAN_POINT('Ctrl Pts',(7.4,3.93840438103015,3.08041733073337));
#38417=CARTESIAN_POINT('',(0.6,3.88328157299975,2.82136921100387));
#38418=CARTESIAN_POINT('',(0.6,3.88328157299975,2.82136921100387));
#38419=CARTESIAN_POINT('',(0.6,3.95328413982768,3.15034434781135));
#38420=CARTESIAN_POINT('Origin',(0.6,3.98440869729662,2.89484236754043));
#38421=CARTESIAN_POINT('',(0.6,3.88328157299975,2.82136921100387));
#38422=CARTESIAN_POINT('Origin',(0.6,3.88328157299975,2.82136921100387));
#38423=CARTESIAN_POINT('Ctrl Pts',(7.4,4.14668485976156,2.79374384542038));
#38424=CARTESIAN_POINT('Ctrl Pts',(7.50357879858679,4.01229542774018,2.80783841969768));
#38425=CARTESIAN_POINT('Ctrl Pts',(7.6,3.88328157299975,2.82136921100387));
#38426=CARTESIAN_POINT('Origin',(0.6,4.52188881640308,2.25956777550238));
#38427=CARTESIAN_POINT('',(7.6,4.38501819668448,1.95233588676384));
#38428=CARTESIAN_POINT('Ctrl Pts',(7.6,4.38501819668449,1.95233588676384));
#38429=CARTESIAN_POINT('Ctrl Pts',(7.50357879858667,4.4378071150503,2.07083055806246));
#38430=CARTESIAN_POINT('Ctrl Pts',(7.4,4.49279557168126,2.19426250733163));
#38431=CARTESIAN_POINT('',(0.6,4.38501819668448,1.95233588676384));
#38432=CARTESIAN_POINT('',(0.6,4.38501819668448,1.95233588676384));
#38433=CARTESIAN_POINT('',(0.6,4.52188881640308,2.25956777550238));
#38434=CARTESIAN_POINT('Origin',(0.6,4.49921137888981,2.00317796714832));
#38435=CARTESIAN_POINT('',(0.6,4.38501819668448,1.95233588676384));
#38436=CARTESIAN_POINT('Origin',(0.6,4.38501819668448,1.95233588676384));
#38437=CARTESIAN_POINT('Ctrl Pts',(7.4,4.63692185318803,1.87054957898135));
#38438=CARTESIAN_POINT('Ctrl Pts',(7.50357879858679,4.5083995794617,1.91227728703365));
#38439=CARTESIAN_POINT('Ctrl Pts',(7.6,4.38501819668448,1.95233588676384));
#38440=CARTESIAN_POINT('Origin',(0.6,4.89286525327172,1.27003724879479));
#38441=CARTESIAN_POINT('',(7.6,4.69510848352227,0.997976115925245));
#38442=CARTESIAN_POINT('Ctrl Pts',(7.6,4.69510848352227,0.997976115925245));
#38443=CARTESIAN_POINT('Ctrl Pts',(7.50357879858677,4.77138026482964,1.10290596108175));
#38444=CARTESIAN_POINT('Ctrl Pts',(7.4,4.85083003702482,1.21220788311979));
#38445=CARTESIAN_POINT('',(0.6,4.69510848352227,0.997976115925245));
#38446=CARTESIAN_POINT('',(0.6,4.69510848352227,0.997976115925245));
#38447=CARTESIAN_POINT('',(0.6,4.89286525327172,1.27003724879479));
#38448=CARTESIAN_POINT('Origin',(0.6,4.81737693361399,1.02396507727746));
#38449=CARTESIAN_POINT('',(0.6,4.69510848352227,0.997976115925245));
#38450=CARTESIAN_POINT('Origin',(0.6,4.69510848352227,0.997976115925245));
#38451=CARTESIAN_POINT('Ctrl Pts',(7.4,4.92450311121048,0.865603320048098));
#38452=CARTESIAN_POINT('Ctrl Pts',(7.50357879858674,4.80746503585938,0.933140460801728));
#38453=CARTESIAN_POINT('Ctrl Pts',(7.6,4.69510848352227,0.997976115925244));
#38454=CARTESIAN_POINT('Origin',(0.6,5.05,0.225));
#38455=CARTESIAN_POINT('',(7.6,4.8,0.));
#38456=CARTESIAN_POINT('Ctrl Pts',(7.6,4.8,5.66922395553271E-16));
#38457=CARTESIAN_POINT('Ctrl Pts',(7.50357879858671,4.89642120141329,0.0867790812719613));
#38458=CARTESIAN_POINT('Ctrl Pts',(7.4,4.99685995288536,0.177173957596824));
#38459=CARTESIAN_POINT('',(0.6,4.8,0.));
#38460=CARTESIAN_POINT('',(0.6,4.8,0.));
#38461=CARTESIAN_POINT('',(0.6,5.05,0.225));
#38462=CARTESIAN_POINT('Origin',(0.6,4.925,0.));
#38463=CARTESIAN_POINT('',(0.6,4.8,0.));
#38464=CARTESIAN_POINT('Origin',(0.6,4.8,0.));
#38465=CARTESIAN_POINT('Ctrl Pts',(7.4,4.99685995288536,-0.177173957596825));
#38466=CARTESIAN_POINT('Ctrl Pts',(7.5035787985867,4.8964212014133,-0.0867790812719661));
#38467=CARTESIAN_POINT('Ctrl Pts',(7.6,4.8,-5.66922395553271E-16));
#38468=CARTESIAN_POINT('Origin',(-12.,2.1,0.));
#38469=CARTESIAN_POINT('',(-12.,-2.1,-2.57175827820944E-16));
#38470=CARTESIAN_POINT('Origin',(-12.,0.,0.));
#38471=CARTESIAN_POINT('Origin',(-11.8,0.,0.));
#38472=CARTESIAN_POINT('',(-11.8,-2.3,-2.81668763803891E-16));
#38473=CARTESIAN_POINT('Origin',(-5.8,0.,0.));
#38474=CARTESIAN_POINT('Origin',(0.,0.,0.));
#38475=CARTESIAN_POINT('Origin',(0.,4.5,0.));
#38476=CARTESIAN_POINT('',(2.08166817117217E-16,-4.5,-5.51091059616309E-16));
#38477=CARTESIAN_POINT('Origin',(0.,0.,0.));
#38478=CARTESIAN_POINT('Origin',(0.25,0.,0.));
#38479=CARTESIAN_POINT('',(0.25,-4.75,-5.81707229594993E-16));
#38480=CARTESIAN_POINT('Origin',(7.7,0.,0.));
#38481=CARTESIAN_POINT('',(8.,-4.4,-5.38844591624835E-16));
#38482=CARTESIAN_POINT('Origin',(8.,0.,0.));
#38483=CARTESIAN_POINT('',(7.7,-4.7,-5.75583995599256E-16));
#38484=CARTESIAN_POINT('Origin',(8.,0.,0.));
#38485=CARTESIAN_POINT('',(0.,0.,0.));
#38486=CARTESIAN_POINT('',(0.,0.,0.));
#38487=CARTESIAN_POINT('',(30.9999999999999,5.96744875736018E-15,22.5));
#38488=CARTESIAN_POINT('',(9.57952682562335,29.4827520051498,22.5));
#38489=CARTESIAN_POINT('',(-25.0795268256234,18.2213428210667,22.5));
#38490=CARTESIAN_POINT('',(-25.0795268256234,-18.2213428210667,22.5));
#38491=CARTESIAN_POINT('',(9.57952682562336,-29.4827520051498,22.5));
#38492=CARTESIAN_POINT('',(0.,0.,0.));
#38493=CARTESIAN_POINT('',(5.55111512312578E-16,3.08148791101957E-32,22.5));
#38494=CARTESIAN_POINT('',(0.,0.,14.));
#38495=CARTESIAN_POINT('',(0.,0.,22.6));
#38496=CARTESIAN_POINT('',(0.,0.,24.2));
#38497=CARTESIAN_POINT('',(16.1803398874989,11.7557050458495,13.1695728752538));
#38498=CARTESIAN_POINT('',(16.1803398874989,11.7557050458495,4.));
#38499=CARTESIAN_POINT('',(16.1803398874989,11.7557050458495,4.));
#38500=CARTESIAN_POINT('',(0.,47.5,5.));
#38501=UNCERTAINTY_MEASURE_WITH_UNIT(LENGTH_MEASURE(0.01),#38529,
'DISTANCE_ACCURACY_VALUE',
'Maximum model space distance between geometric entities at asserted c
onnectivities');
#38502=UNCERTAINTY_MEASURE_WITH_UNIT(LENGTH_MEASURE(0.01),#38529,
'DISTANCE_ACCURACY_VALUE',
'Maximum model space distance between geometric entities at asserted c
onnectivities');
#38503=UNCERTAINTY_MEASURE_WITH_UNIT(LENGTH_MEASURE(0.01),#38529,
'DISTANCE_ACCURACY_VALUE',
'Maximum model space distance between geometric entities at asserted c
onnectivities');
#38504=UNCERTAINTY_MEASURE_WITH_UNIT(LENGTH_MEASURE(0.01),#38529,
'DISTANCE_ACCURACY_VALUE',
'Maximum model space distance between geometric entities at asserted c
onnectivities');
#38505=UNCERTAINTY_MEASURE_WITH_UNIT(LENGTH_MEASURE(0.01),#38529,
'DISTANCE_ACCURACY_VALUE',
'Maximum model space distance between geometric entities at asserted c
onnectivities');
#38506=UNCERTAINTY_MEASURE_WITH_UNIT(LENGTH_MEASURE(0.01),#38529,
'DISTANCE_ACCURACY_VALUE',
'Maximum model space distance between geometric entities at asserted c
onnectivities');
#38507=UNCERTAINTY_MEASURE_WITH_UNIT(LENGTH_MEASURE(0.01),#38529,
'DISTANCE_ACCURACY_VALUE',
'Maximum model space distance between geometric entities at asserted c
onnectivities');
#38508=UNCERTAINTY_MEASURE_WITH_UNIT(LENGTH_MEASURE(0.01),#38529,
'DISTANCE_ACCURACY_VALUE',
'Maximum model space distance between geometric entities at asserted c
onnectivities');
#38509=UNCERTAINTY_MEASURE_WITH_UNIT(LENGTH_MEASURE(0.01),#38529,
'DISTANCE_ACCURACY_VALUE',
'Maximum model space distance between geometric entities at asserted c
onnectivities');
#38510=UNCERTAINTY_MEASURE_WITH_UNIT(LENGTH_MEASURE(0.01),#38529,
'DISTANCE_ACCURACY_VALUE',
'Maximum model space distance between geometric entities at asserted c
onnectivities');
#38511=UNCERTAINTY_MEASURE_WITH_UNIT(LENGTH_MEASURE(0.01),#38529,
'DISTANCE_ACCURACY_VALUE',
'Maximum model space distance between geometric entities at asserted c
onnectivities');
#38512=UNCERTAINTY_MEASURE_WITH_UNIT(LENGTH_MEASURE(0.01),#38529,
'DISTANCE_ACCURACY_VALUE',
'Maximum model space distance between geometric entities at asserted c
onnectivities');
#38513=UNCERTAINTY_MEASURE_WITH_UNIT(LENGTH_MEASURE(0.01),#38529,
'DISTANCE_ACCURACY_VALUE',
'Maximum model space distance between geometric entities at asserted c
onnectivities');
#38514=UNCERTAINTY_MEASURE_WITH_UNIT(LENGTH_MEASURE(0.01),#38529,
'DISTANCE_ACCURACY_VALUE',
'Maximum model space distance between geometric entities at asserted c
onnectivities');
#38515=(
GEOMETRIC_REPRESENTATION_CONTEXT(3)
GLOBAL_UNCERTAINTY_ASSIGNED_CONTEXT((#38501))
GLOBAL_UNIT_ASSIGNED_CONTEXT((#38529,#38531,#38532))
REPRESENTATION_CONTEXT('','3D')
);
#38516=(
GEOMETRIC_REPRESENTATION_CONTEXT(3)
GLOBAL_UNCERTAINTY_ASSIGNED_CONTEXT((#38502))
GLOBAL_UNIT_ASSIGNED_CONTEXT((#38529,#38531,#38532))
REPRESENTATION_CONTEXT('','3D')
);
#38517=(
GEOMETRIC_REPRESENTATION_CONTEXT(3)
GLOBAL_UNCERTAINTY_ASSIGNED_CONTEXT((#38503))
GLOBAL_UNIT_ASSIGNED_CONTEXT((#38529,#38531,#38532))
REPRESENTATION_CONTEXT('','3D')
);
#38518=(
GEOMETRIC_REPRESENTATION_CONTEXT(3)
GLOBAL_UNCERTAINTY_ASSIGNED_CONTEXT((#38504))
GLOBAL_UNIT_ASSIGNED_CONTEXT((#38529,#38531,#38532))
REPRESENTATION_CONTEXT('','3D')
);
#38519=(
GEOMETRIC_REPRESENTATION_CONTEXT(3)
GLOBAL_UNCERTAINTY_ASSIGNED_CONTEXT((#38505))
GLOBAL_UNIT_ASSIGNED_CONTEXT((#38529,#38531,#38532))
REPRESENTATION_CONTEXT('','3D')
);
#38520=(
GEOMETRIC_REPRESENTATION_CONTEXT(3)
GLOBAL_UNCERTAINTY_ASSIGNED_CONTEXT((#38506))
GLOBAL_UNIT_ASSIGNED_CONTEXT((#38529,#38531,#38532))
REPRESENTATION_CONTEXT('','3D')
);
#38521=(
GEOMETRIC_REPRESENTATION_CONTEXT(3)
GLOBAL_UNCERTAINTY_ASSIGNED_CONTEXT((#38507))
GLOBAL_UNIT_ASSIGNED_CONTEXT((#38529,#38531,#38532))
REPRESENTATION_CONTEXT('','3D')
);
#38522=(
GEOMETRIC_REPRESENTATION_CONTEXT(3)
GLOBAL_UNCERTAINTY_ASSIGNED_CONTEXT((#38508))
GLOBAL_UNIT_ASSIGNED_CONTEXT((#38529,#38531,#38532))
REPRESENTATION_CONTEXT('','3D')
);
#38523=(
GEOMETRIC_REPRESENTATION_CONTEXT(3)
GLOBAL_UNCERTAINTY_ASSIGNED_CONTEXT((#38509))
GLOBAL_UNIT_ASSIGNED_CONTEXT((#38529,#38531,#38532))
REPRESENTATION_CONTEXT('','3D')
);
#38524=(
GEOMETRIC_REPRESENTATION_CONTEXT(3)
GLOBAL_UNCERTAINTY_ASSIGNED_CONTEXT((#38510))
GLOBAL_UNIT_ASSIGNED_CONTEXT((#38529,#38531,#38532))
REPRESENTATION_CONTEXT('','3D')
);
#38525=(
GEOMETRIC_REPRESENTATION_CONTEXT(3)
GLOBAL_UNCERTAINTY_ASSIGNED_CONTEXT((#38511))
GLOBAL_UNIT_ASSIGNED_CONTEXT((#38529,#38531,#38532))
REPRESENTATION_CONTEXT('','3D')
);
#38526=(
GEOMETRIC_REPRESENTATION_CONTEXT(3)
GLOBAL_UNCERTAINTY_ASSIGNED_CONTEXT((#38512))
GLOBAL_UNIT_ASSIGNED_CONTEXT((#38529,#38531,#38532))
REPRESENTATION_CONTEXT('','3D')
);
#38527=(
GEOMETRIC_REPRESENTATION_CONTEXT(3)
GLOBAL_UNCERTAINTY_ASSIGNED_CONTEXT((#38513))
GLOBAL_UNIT_ASSIGNED_CONTEXT((#38529,#38531,#38532))
REPRESENTATION_CONTEXT('','3D')
);
#38528=(
GEOMETRIC_REPRESENTATION_CONTEXT(3)
GLOBAL_UNCERTAINTY_ASSIGNED_CONTEXT((#38514))
GLOBAL_UNIT_ASSIGNED_CONTEXT((#38529,#38531,#38532))
REPRESENTATION_CONTEXT('','3D')
);
#38529=(
LENGTH_UNIT()
NAMED_UNIT(*)
SI_UNIT(.MILLI.,.METRE.)
);
#38530=(
LENGTH_UNIT()
NAMED_UNIT(*)
SI_UNIT($,.METRE.)
);
#38531=(
NAMED_UNIT(*)
PLANE_ANGLE_UNIT()
SI_UNIT($,.RADIAN.)
);
#38532=(
NAMED_UNIT(*)
SI_UNIT($,.STERADIAN.)
SOLID_ANGLE_UNIT()
);
#38533=SHAPE_DEFINITION_REPRESENTATION(#38546,#38575);
#38534=SHAPE_DEFINITION_REPRESENTATION(#38547,#38576);
#38535=SHAPE_DEFINITION_REPRESENTATION(#38548,#38577);
#38536=SHAPE_DEFINITION_REPRESENTATION(#38549,#38578);
#38537=SHAPE_DEFINITION_REPRESENTATION(#38550,#38579);
#38538=SHAPE_DEFINITION_REPRESENTATION(#38551,#38580);
#38539=SHAPE_DEFINITION_REPRESENTATION(#38552,#38581);
#38540=SHAPE_DEFINITION_REPRESENTATION(#38553,#38582);
#38541=SHAPE_DEFINITION_REPRESENTATION(#38554,#38583);
#38542=SHAPE_DEFINITION_REPRESENTATION(#38555,#38584);
#38543=SHAPE_DEFINITION_REPRESENTATION(#38556,#38585);
#38544=SHAPE_DEFINITION_REPRESENTATION(#38557,#38586);
#38545=SHAPE_DEFINITION_REPRESENTATION(#38558,#38587);
#38546=PRODUCT_DEFINITION_SHAPE('',$,#38589);
#38547=PRODUCT_DEFINITION_SHAPE('',$,#38590);
#38548=PRODUCT_DEFINITION_SHAPE('',$,#38591);
#38549=PRODUCT_DEFINITION_SHAPE('',$,#38592);
#38550=PRODUCT_DEFINITION_SHAPE('',$,#38593);
#38551=PRODUCT_DEFINITION_SHAPE('',$,#38594);
#38552=PRODUCT_DEFINITION_SHAPE('',$,#38595);
#38553=PRODUCT_DEFINITION_SHAPE('',$,#38596);
#38554=PRODUCT_DEFINITION_SHAPE('',$,#38597);
#38555=PRODUCT_DEFINITION_SHAPE('',$,#38598);
#38556=PRODUCT_DEFINITION_SHAPE('',$,#38599);
#38557=PRODUCT_DEFINITION_SHAPE('',$,#38600);
#38558=PRODUCT_DEFINITION_SHAPE('',$,#38601);
#38559=PRODUCT_DEFINITION_SHAPE($,$,#59);
#38560=PRODUCT_DEFINITION_SHAPE($,$,#60);
#38561=PRODUCT_DEFINITION_SHAPE($,$,#61);
#38562=PRODUCT_DEFINITION_SHAPE($,$,#62);
#38563=PRODUCT_DEFINITION_SHAPE($,$,#63);
#38564=PRODUCT_DEFINITION_SHAPE($,$,#64);
#38565=PRODUCT_DEFINITION_SHAPE($,$,#65);
#38566=PRODUCT_DEFINITION_SHAPE($,$,#66);
#38567=PRODUCT_DEFINITION_SHAPE($,$,#67);
#38568=PRODUCT_DEFINITION_SHAPE($,$,#68);
#38569=PRODUCT_DEFINITION_SHAPE($,$,#69);
#38570=PRODUCT_DEFINITION_SHAPE($,$,#70);
#38571=PRODUCT_DEFINITION_SHAPE($,$,#71);
#38572=PRODUCT_DEFINITION_SHAPE($,$,#72);
#38573=PRODUCT_DEFINITION_SHAPE($,$,#73);
#38574=PRODUCT_DEFINITION_SHAPE($,$,#74);
#38575=SHAPE_REPRESENTATION('',(#17217,#19009,#19010,#19011,#19012,#19013,
#19014,#19015,#19016,#19017,#19018,#19019,#19020,#19021,#19022,#19023,#19024),
#38515);
#38576=SHAPE_REPRESENTATION('',(#17218),#38516);
#38577=SHAPE_REPRESENTATION('',(#17323),#38517);
#38578=SHAPE_REPRESENTATION('',(#18599),#38518);
#38579=SHAPE_REPRESENTATION('',(#18641),#38519);
#38580=SHAPE_REPRESENTATION('',(#18673),#38520);
#38581=SHAPE_REPRESENTATION('',(#18699),#38521);
#38582=SHAPE_REPRESENTATION('',(#18708),#38522);
#38583=SHAPE_REPRESENTATION('',(#18722),#38523);
#38584=SHAPE_REPRESENTATION('',(#18766),#38524);
#38585=SHAPE_REPRESENTATION('',(#18769),#38525);
#38586=SHAPE_REPRESENTATION('',(#18774),#38526);
#38587=SHAPE_REPRESENTATION('',(#18808),#38527);
#38588=PRODUCT_DEFINITION_CONTEXT('part definition',#38629,'design');
#38589=PRODUCT_DEFINITION('2026-10-20-13-39-02-152','MAS-288',#38602,#38588);
#38590=PRODUCT_DEFINITION('2026-10-20-13-39-03-241',
'01_Turret_Base_with_Dovetail',#38603,#38588);
#38591=PRODUCT_DEFINITION('2026-10-20-13-39-04-258',
'02_Revolving_Objective_Disc_D107',#38604,#38588);
#38592=PRODUCT_DEFINITION('2026-10-20-13-39-07-742',
'03_Brass_RMS_Objective_Socket',#38605,#38588);
#38593=PRODUCT_DEFINITION('2026-10-20-13-39-08-151',
'04_Central_Spindle_D10_M6',#38606,#38588);
#38594=PRODUCT_DEFINITION('2026-10-20-13-39-08-542','05_Centre_Cap',#38607,
#38588);
#38595=PRODUCT_DEFINITION('2026-10-20-13-39-09-036',
'06_PTFE_Thrust_Washer_24x10.5x0.5',#38608,#38588);
#38596=PRODUCT_DEFINITION('2026-10-20-13-39-09-288',
'07_ISO_7089_Washer_M6',#38609,#38588);
#38597=PRODUCT_DEFINITION('2026-10-20-13-39-09-546',
'08_ISO_4032_Nut_M6',#38610,#38588);
#38598=PRODUCT_DEFINITION('2026-10-20-13-39-10-336',
'09_Detent_Ball_D4_Hardened',#38611,#38588);
#38599=PRODUCT_DEFINITION('2026-10-20-13-39-10-551',
'10_Detent_Spring_D3.8',#38612,#38588);
#38600=PRODUCT_DEFINITION('2026-10-20-13-39-11-796',
'11_ISO_4026_Set_Screw_M5x4',#38613,#38588);
#38601=PRODUCT_DEFINITION('2026-10-20-13-39-12-626',
'12_Dovetail_Lock_Thumb_Screw_M5',#38614,#38588);
#38602=PRODUCT_DEFINITION_FORMATION('',$,#38631);
#38603=PRODUCT_DEFINITION_FORMATION('',$,#38632);
#38604=PRODUCT_DEFINITION_FORMATION('',$,#38633);
#38605=PRODUCT_DEFINITION_FORMATION('',$,#38634);
#38606=PRODUCT_DEFINITION_FORMATION('',$,#38635);
#38607=PRODUCT_DEFINITION_FORMATION('',$,#38636);
#38608=PRODUCT_DEFINITION_FORMATION('',$,#38637);
#38609=PRODUCT_DEFINITION_FORMATION('',$,#38638);
#38610=PRODUCT_DEFINITION_FORMATION('',$,#38639);
#38611=PRODUCT_DEFINITION_FORMATION('',$,#38640);
#38612=PRODUCT_DEFINITION_FORMATION('',$,#38641);
#38613=PRODUCT_DEFINITION_FORMATION('',$,#38642);
#38614=PRODUCT_DEFINITION_FORMATION('',$,#38643);
#38615=PRODUCT_RELATED_PRODUCT_CATEGORY('MAS-288','MAS-288',(#38631));
#38616=PRODUCT_RELATED_PRODUCT_CATEGORY('01_Turret_Base_with_Dovetail',
'01_Turret_Base_with_Dovetail',(#38632));
#38617=PRODUCT_RELATED_PRODUCT_CATEGORY(
'02_Revolving_Objective_Disc_D107','02_Revolving_Objective_Disc_D107',(#38633));
#38618=PRODUCT_RELATED_PRODUCT_CATEGORY('03_Brass_RMS_Objective_Socket',
'03_Brass_RMS_Objective_Socket',(#38634));
#38619=PRODUCT_RELATED_PRODUCT_CATEGORY('04_Central_Spindle_D10_M6',
'04_Central_Spindle_D10_M6',(#38635));
#38620=PRODUCT_RELATED_PRODUCT_CATEGORY('05_Centre_Cap','05_Centre_Cap',
(#38636));
#38621=PRODUCT_RELATED_PRODUCT_CATEGORY(
'06_PTFE_Thrust_Washer_24x10.5x0.5','06_PTFE_Thrust_Washer_24x10.5x0.5',
(#38637));
#38622=PRODUCT_RELATED_PRODUCT_CATEGORY('07_ISO_7089_Washer_M6',
'07_ISO_7089_Washer_M6',(#38638));
#38623=PRODUCT_RELATED_PRODUCT_CATEGORY('08_ISO_4032_Nut_M6',
'08_ISO_4032_Nut_M6',(#38639));
#38624=PRODUCT_RELATED_PRODUCT_CATEGORY('09_Detent_Ball_D4_Hardened',
'09_Detent_Ball_D4_Hardened',(#38640));
#38625=PRODUCT_RELATED_PRODUCT_CATEGORY('10_Detent_Spring_D3.8',
'10_Detent_Spring_D3.8',(#38641));
#38626=PRODUCT_RELATED_PRODUCT_CATEGORY('11_ISO_4026_Set_Screw_M5x4',
'11_ISO_4026_Set_Screw_M5x4',(#38642));
#38627=PRODUCT_RELATED_PRODUCT_CATEGORY(
'12_Dovetail_Lock_Thumb_Screw_M5','12_Dovetail_Lock_Thumb_Screw_M5',(#38643));
#38628=APPLICATION_PROTOCOL_DEFINITION('international standard',
'automotive_design',2009,#38629);
#38629=APPLICATION_CONTEXT(
'Core Data for Automotive Mechanical Design Process');
#38630=PRODUCT_CONTEXT('part definition',#38629,'mechanical');
#38631=PRODUCT('2026-10-20-13-39-02-152','MAS-288',$,(#38630));
#38632=PRODUCT('2026-10-20-13-39-03-241','01_Turret_Base_with_Dovetail',
$,(#38630));
#38633=PRODUCT('2026-10-20-13-39-04-258',
'02_Revolving_Objective_Disc_D107',$,(#38630));
#38634=PRODUCT('2026-10-20-13-39-07-742',
'03_Brass_RMS_Objective_Socket',$,(#38630));
#38635=PRODUCT('2026-10-20-13-39-08-151','04_Central_Spindle_D10_M6',$,
(#38630));
#38636=PRODUCT('2026-10-20-13-39-08-542','05_Centre_Cap',$,(#38630));
#38637=PRODUCT('2026-10-20-13-39-09-036',
'06_PTFE_Thrust_Washer_24x10.5x0.5',$,(#38630));
#38638=PRODUCT('2026-10-20-13-39-09-288','07_ISO_7089_Washer_M6',$,(#38630));
#38639=PRODUCT('2026-10-20-13-39-09-546','08_ISO_4032_Nut_M6',$,(#38630));
#38640=PRODUCT('2026-10-20-13-39-10-336','09_Detent_Ball_D4_Hardened',$,
(#38630));
#38641=PRODUCT('2026-10-20-13-39-10-551','10_Detent_Spring_D3.8',$,(#38630));
#38642=PRODUCT('2026-10-20-13-39-11-796','11_ISO_4026_Set_Screw_M5x4',$,
(#38630));
#38643=PRODUCT('2026-10-20-13-39-12-626',
'12_Dovetail_Lock_Thumb_Screw_M5',$,(#38630));
#38644=PRESENTATION_STYLE_ASSIGNMENT((#38649));
#38645=PRESENTATION_STYLE_ASSIGNMENT((#38650));
#38646=PRESENTATION_STYLE_ASSIGNMENT((#38651));
#38647=PRESENTATION_STYLE_ASSIGNMENT((#38652));
#38648=PRESENTATION_STYLE_ASSIGNMENT((#38653));
#38649=SURFACE_STYLE_USAGE(.BOTH.,#38654);
#38650=SURFACE_STYLE_USAGE(.BOTH.,#38655);
#38651=SURFACE_STYLE_USAGE(.BOTH.,#38656);
#38652=SURFACE_STYLE_USAGE(.BOTH.,#38657);
#38653=SURFACE_STYLE_USAGE(.BOTH.,#38658);
#38654=SURFACE_SIDE_STYLE('',(#38659));
#38655=SURFACE_SIDE_STYLE('',(#38660));
#38656=SURFACE_SIDE_STYLE('',(#38661));
#38657=SURFACE_SIDE_STYLE('',(#38662));
#38658=SURFACE_SIDE_STYLE('',(#38663));
#38659=SURFACE_STYLE_FILL_AREA(#38664);
#38660=SURFACE_STYLE_FILL_AREA(#38665);
#38661=SURFACE_STYLE_FILL_AREA(#38666);
#38662=SURFACE_STYLE_FILL_AREA(#38667);
#38663=SURFACE_STYLE_FILL_AREA(#38668);
#38664=FILL_AREA_STYLE('Steel - Satin',(#38669));
#38665=FILL_AREA_STYLE('MAS288_gun',(#38670));
#38666=FILL_AREA_STYLE('MAS288_ti',(#38671));
#38667=FILL_AREA_STYLE('MAS288_al',(#38672));
#38668=FILL_AREA_STYLE('MAS288_ss',(#38673));
#38669=FILL_AREA_STYLE_COLOUR('Steel - Satin',#38674);
#38670=FILL_AREA_STYLE_COLOUR('MAS288_gun',#38675);
#38671=FILL_AREA_STYLE_COLOUR('MAS288_ti',#38676);
#38672=FILL_AREA_STYLE_COLOUR('MAS288_al',#38677);
#38673=FILL_AREA_STYLE_COLOUR('MAS288_ss',#38678);
#38674=COLOUR_RGB('Steel - Satin',0.627450980392157,0.627450980392157,0.627450980392157);
#38675=COLOUR_RGB('MAS288_gun',0.313725490196078,0.337254901960784,0.364705882352941);
#38676=COLOUR_RGB('MAS288_ti',0.549019607843137,0.572549019607843,0.596078431372549);
#38677=COLOUR_RGB('MAS288_al',0.67843137254902,0.705882352941177,0.729411764705882);
#38678=COLOUR_RGB('MAS288_ss',0.83921568627451,0.850980392156863,0.862745098039216);
#38679=COLOUR_RGB('Dark Blue',0.08,0.2,0.34);
#38680=FILL_AREA_STYLE_COLOUR('',#38679);
#38681=FILL_AREA_STYLE('',(#38680));
#38682=SURFACE_STYLE_FILL_AREA(#38681);
#38683=SURFACE_SIDE_STYLE('',(#38682));
#38684=SURFACE_STYLE_USAGE(.BOTH.,#38683);
#38685=PRESENTATION_STYLE_ASSIGNMENT((#38684));
#38686=COLOUR_RGB('Light Blue',0.38,0.62,0.78);
#38687=FILL_AREA_STYLE_COLOUR('',#38686);
#38688=FILL_AREA_STYLE('',(#38687));
#38689=SURFACE_STYLE_FILL_AREA(#38688);
#38690=SURFACE_SIDE_STYLE('',(#38689));
#38691=SURFACE_STYLE_USAGE(.BOTH.,#38690);
#38692=PRESENTATION_STYLE_ASSIGNMENT((#38691));
#38693=COLOUR_RGB('Sky Blue',0.24,0.69,0.87);
#38694=FILL_AREA_STYLE_COLOUR('',#38693);
#38695=FILL_AREA_STYLE('',(#38694));
#38696=SURFACE_STYLE_FILL_AREA(#38695);
#38697=SURFACE_SIDE_STYLE('',(#38696));
#38698=SURFACE_STYLE_USAGE(.BOTH.,#38697);
#38699=PRESENTATION_STYLE_ASSIGNMENT((#38698));
#38700=COLOUR_RGB('Grey',0.48,0.52,0.57);
#38701=FILL_AREA_STYLE_COLOUR('',#38700);
#38702=FILL_AREA_STYLE('',(#38701));
#38703=SURFACE_STYLE_FILL_AREA(#38702);
#38704=SURFACE_SIDE_STYLE('',(#38703));
#38705=SURFACE_STYLE_USAGE(.BOTH.,#38704);
#38706=PRESENTATION_STYLE_ASSIGNMENT((#38705));
#38707=COLOUR_RGB('Black',0.12,0.14,0.17);
#38708=FILL_AREA_STYLE_COLOUR('',#38707);
#38709=FILL_AREA_STYLE('',(#38708));
#38710=SURFACE_STYLE_FILL_AREA(#38709);
#38711=SURFACE_SIDE_STYLE('',(#38710));
#38712=SURFACE_STYLE_USAGE(.BOTH.,#38711);
#38713=PRESENTATION_STYLE_ASSIGNMENT((#38712));
#38714=COLOUR_RGB('Off White',0.89,0.88,0.83);
#38715=FILL_AREA_STYLE_COLOUR('',#38714);
#38716=FILL_AREA_STYLE('',(#38715));
#38717=SURFACE_STYLE_FILL_AREA(#38716);
#38718=SURFACE_SIDE_STYLE('',(#38717));
#38719=SURFACE_STYLE_USAGE(.BOTH.,#38718);
#38720=PRESENTATION_STYLE_ASSIGNMENT((#38719));
ENDSEC;
END-ISO-10303-21;
